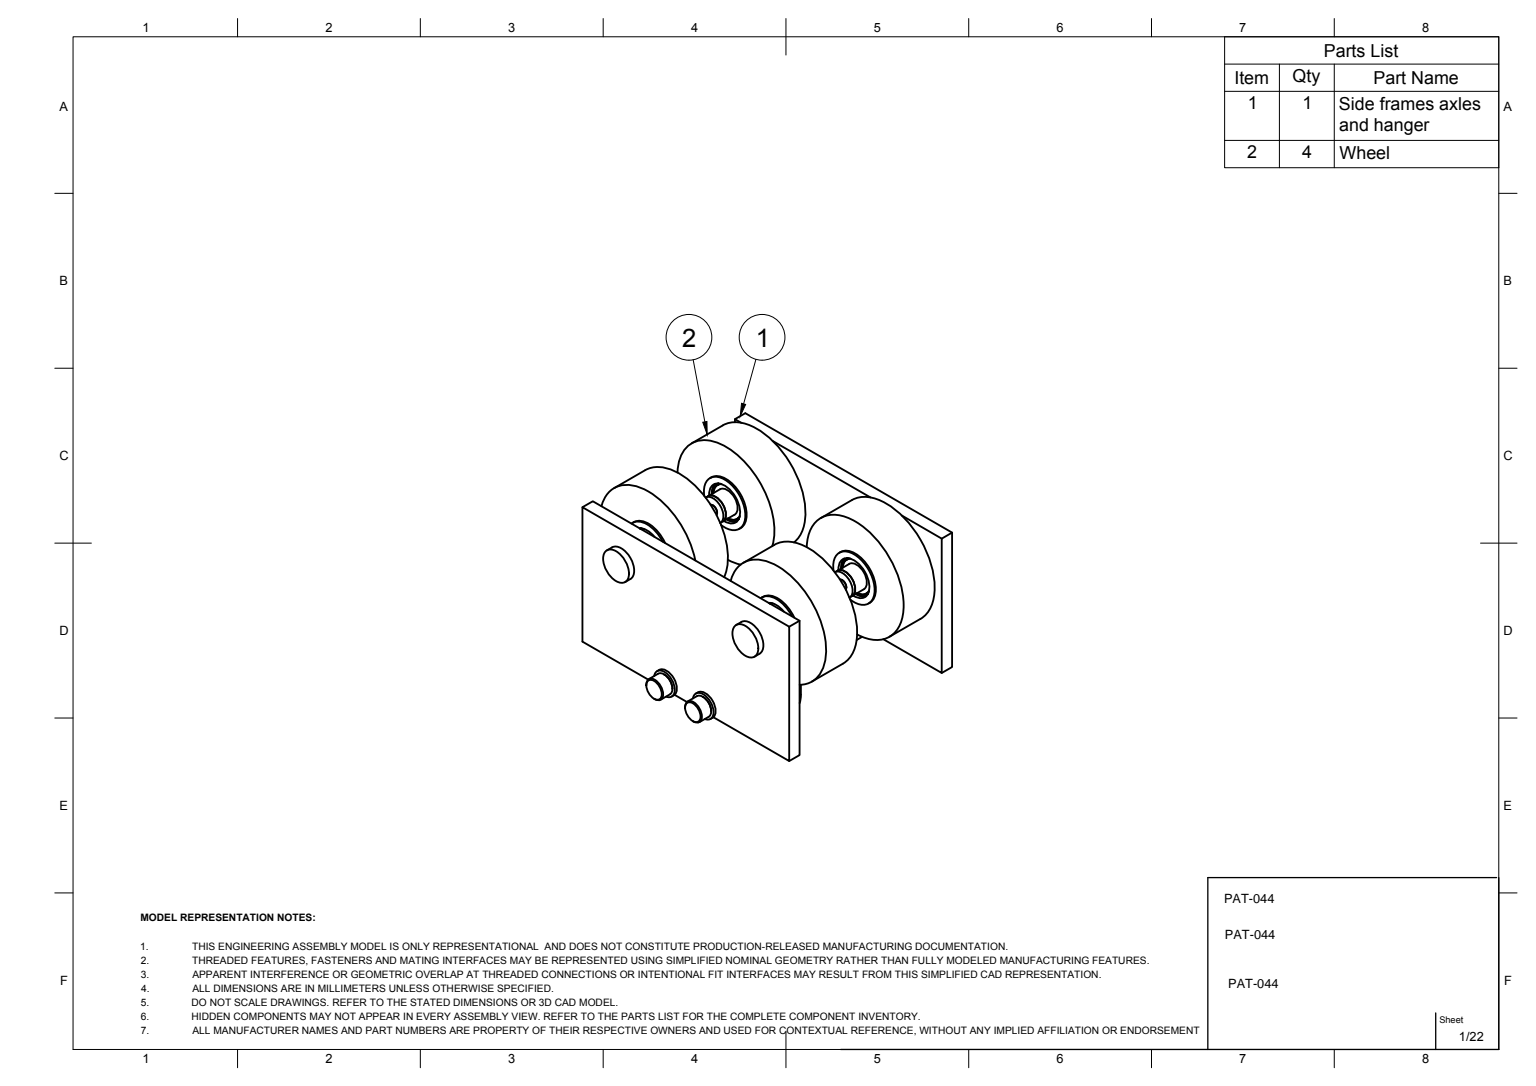
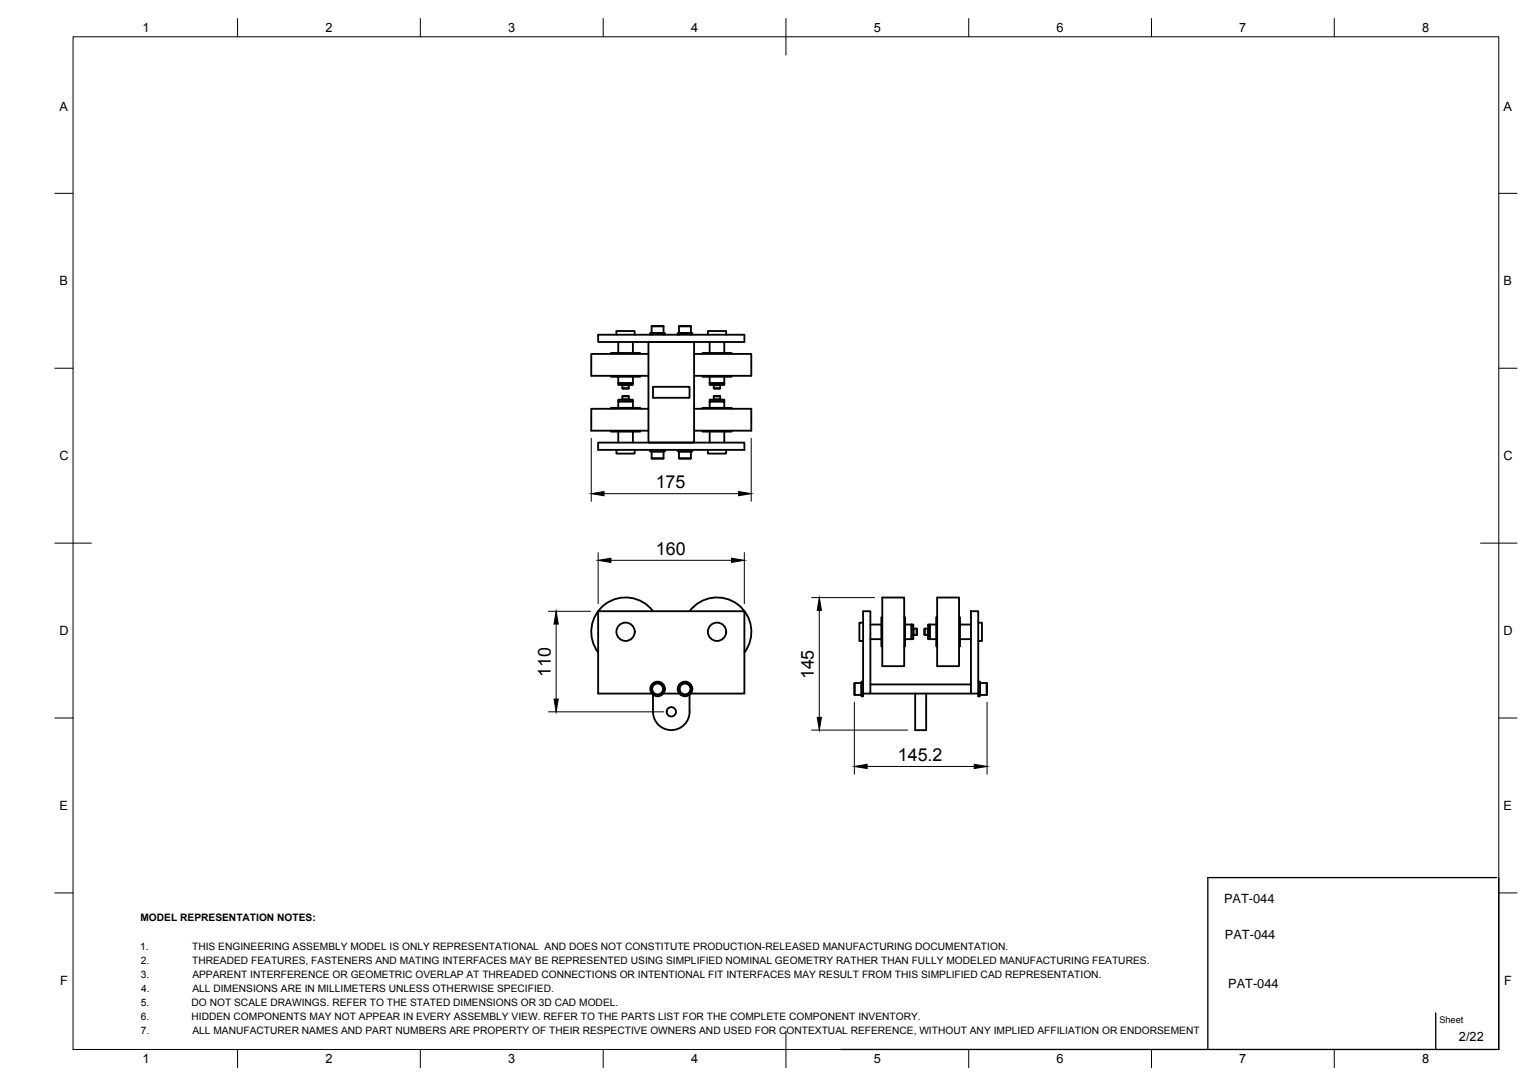
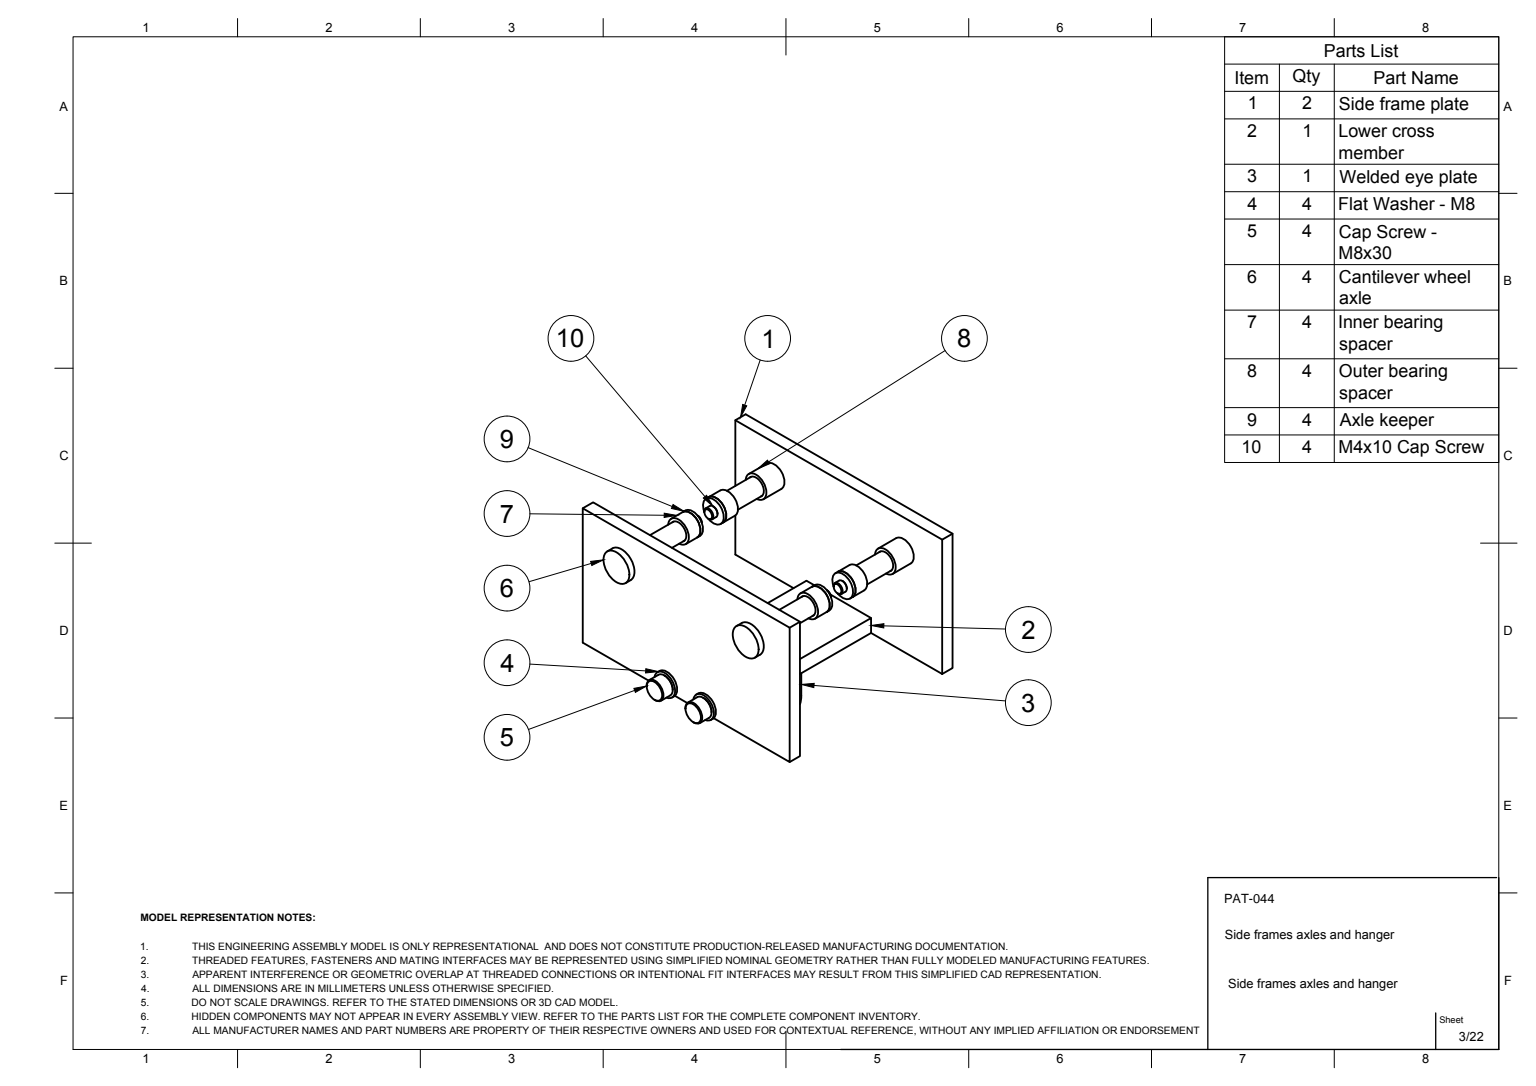
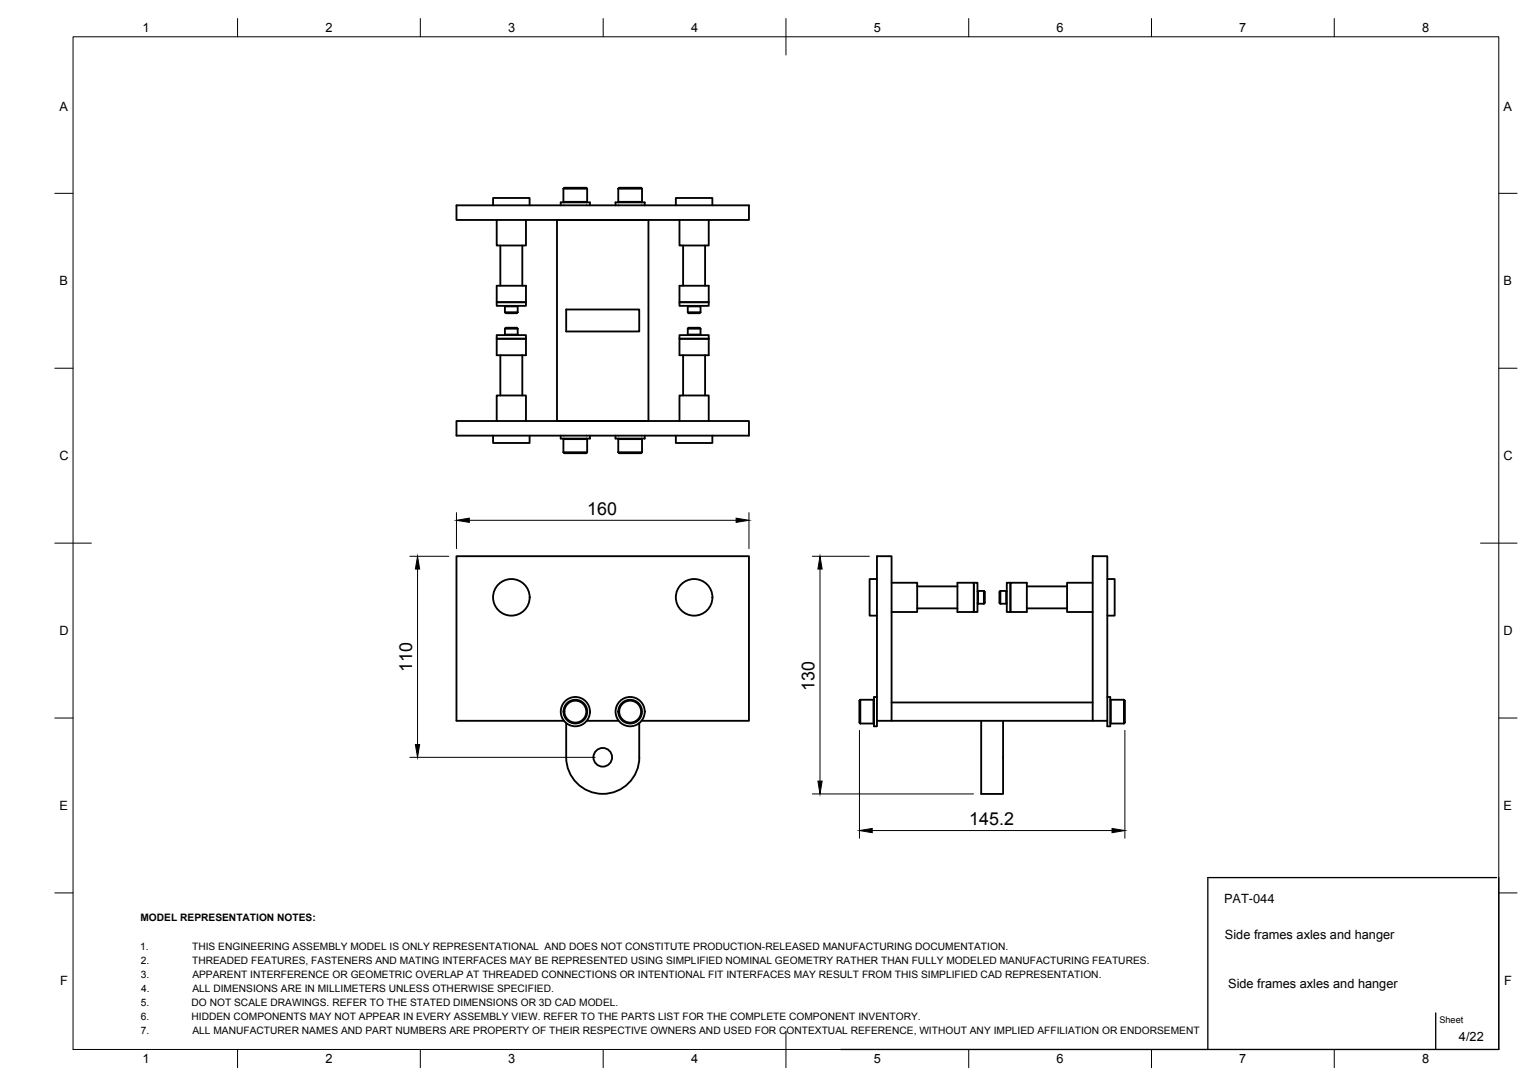
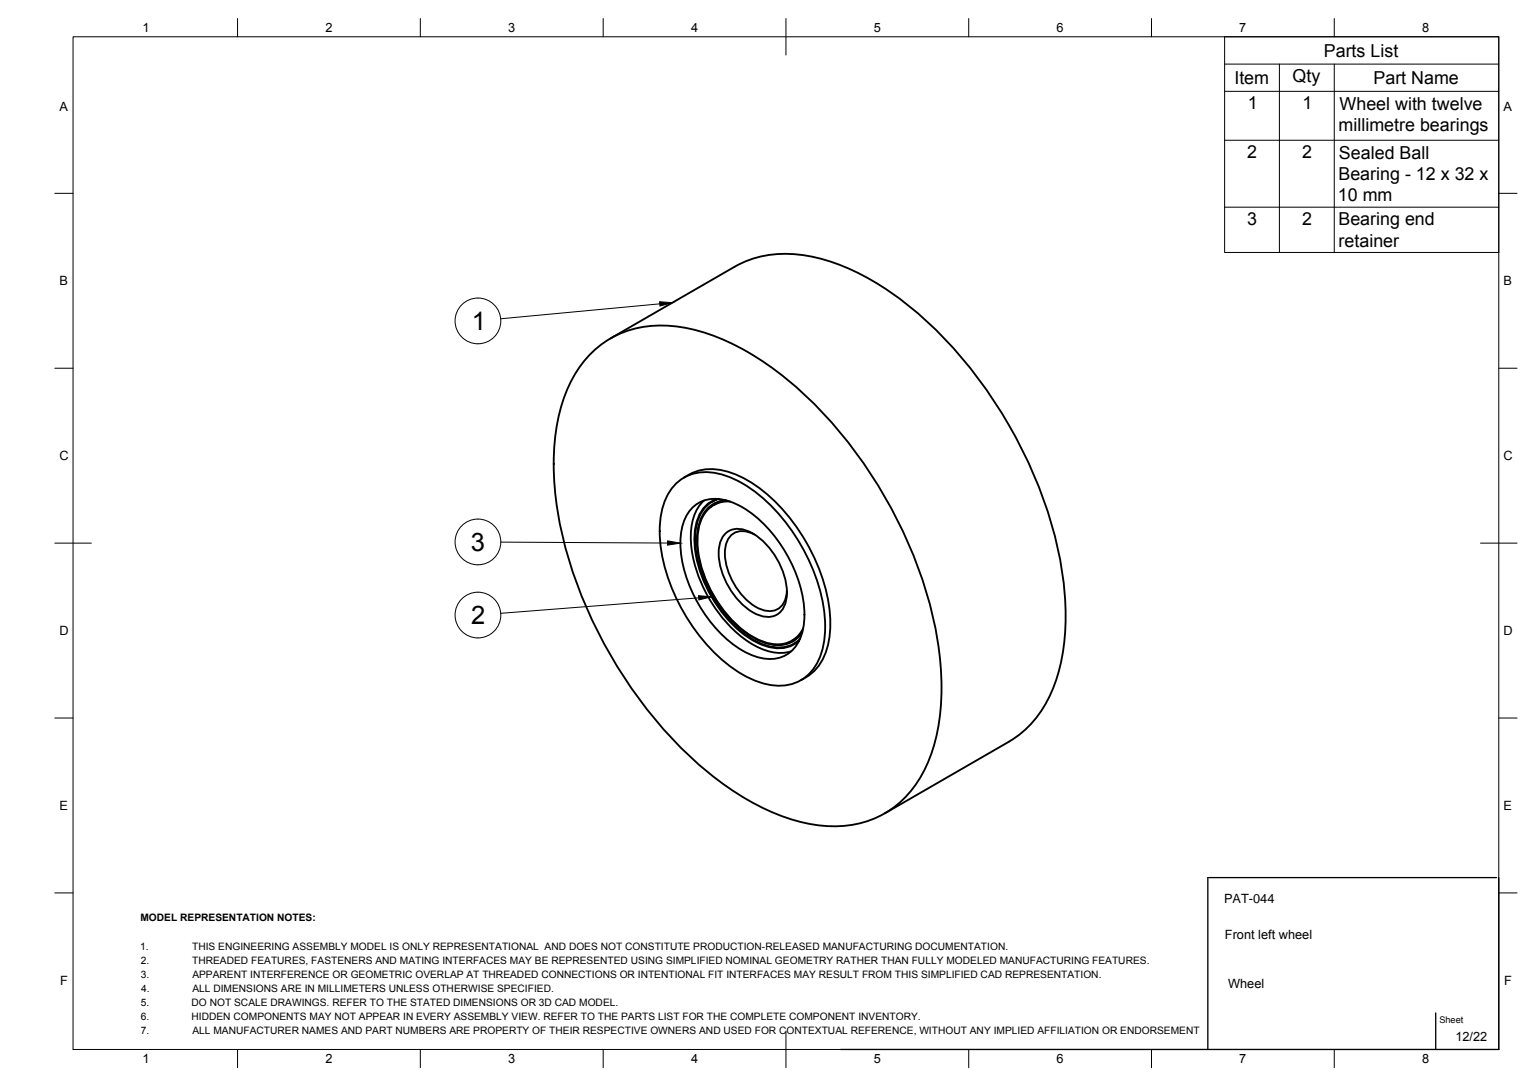
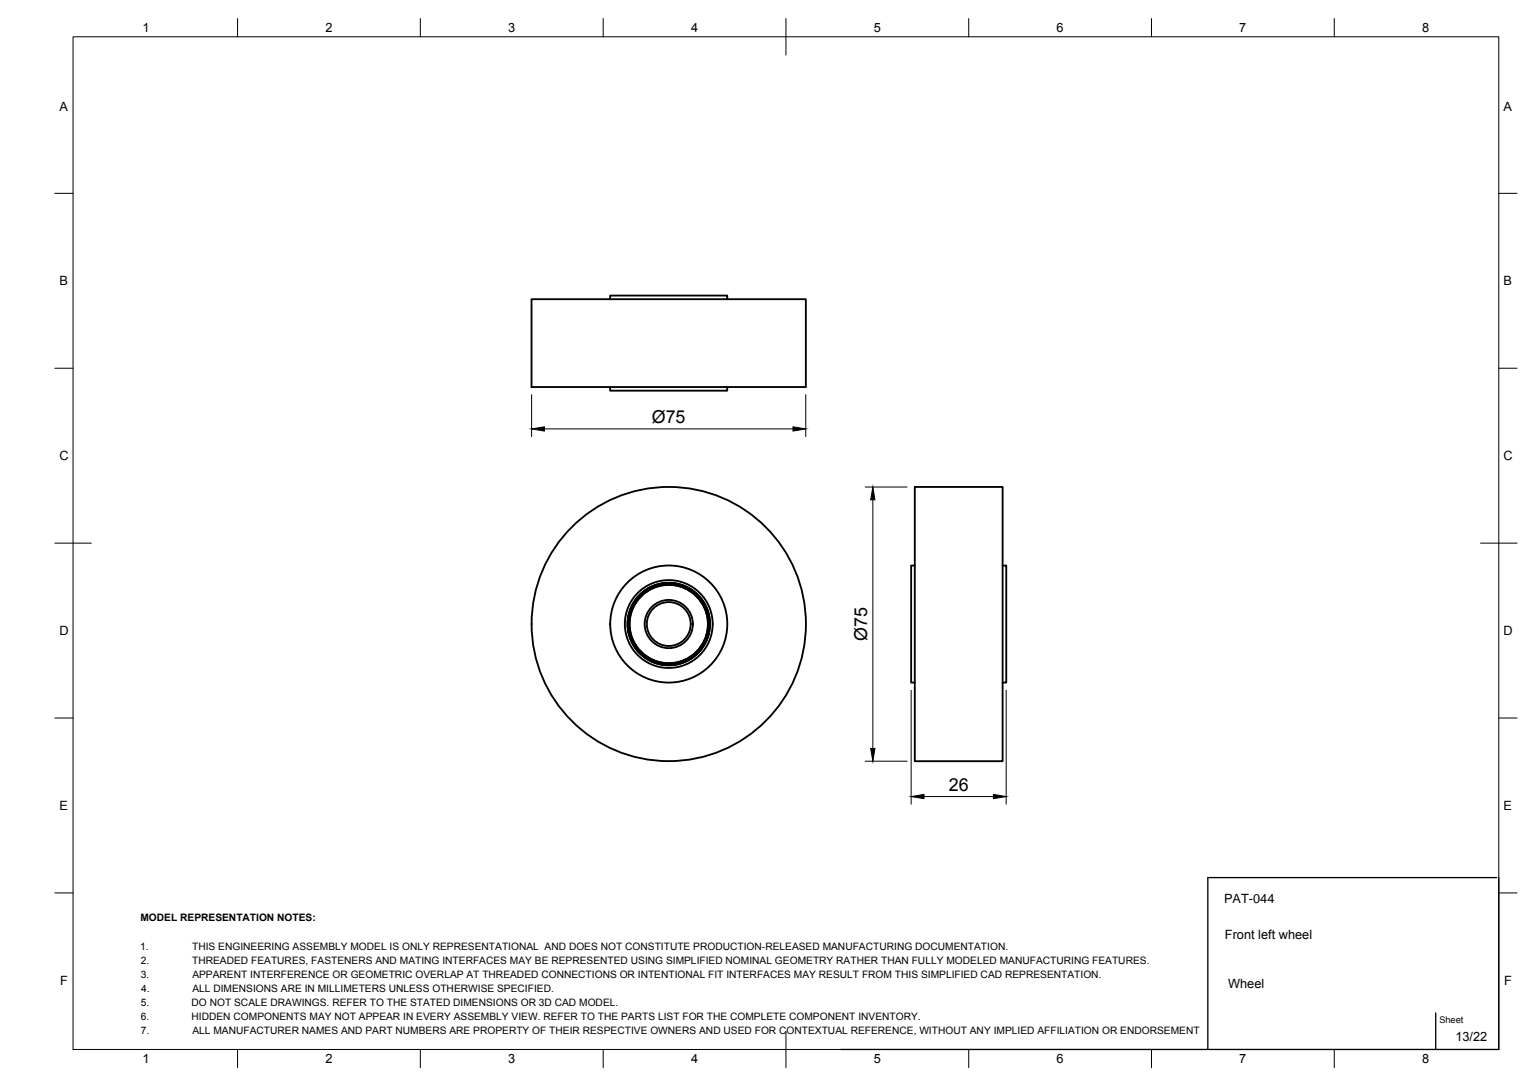
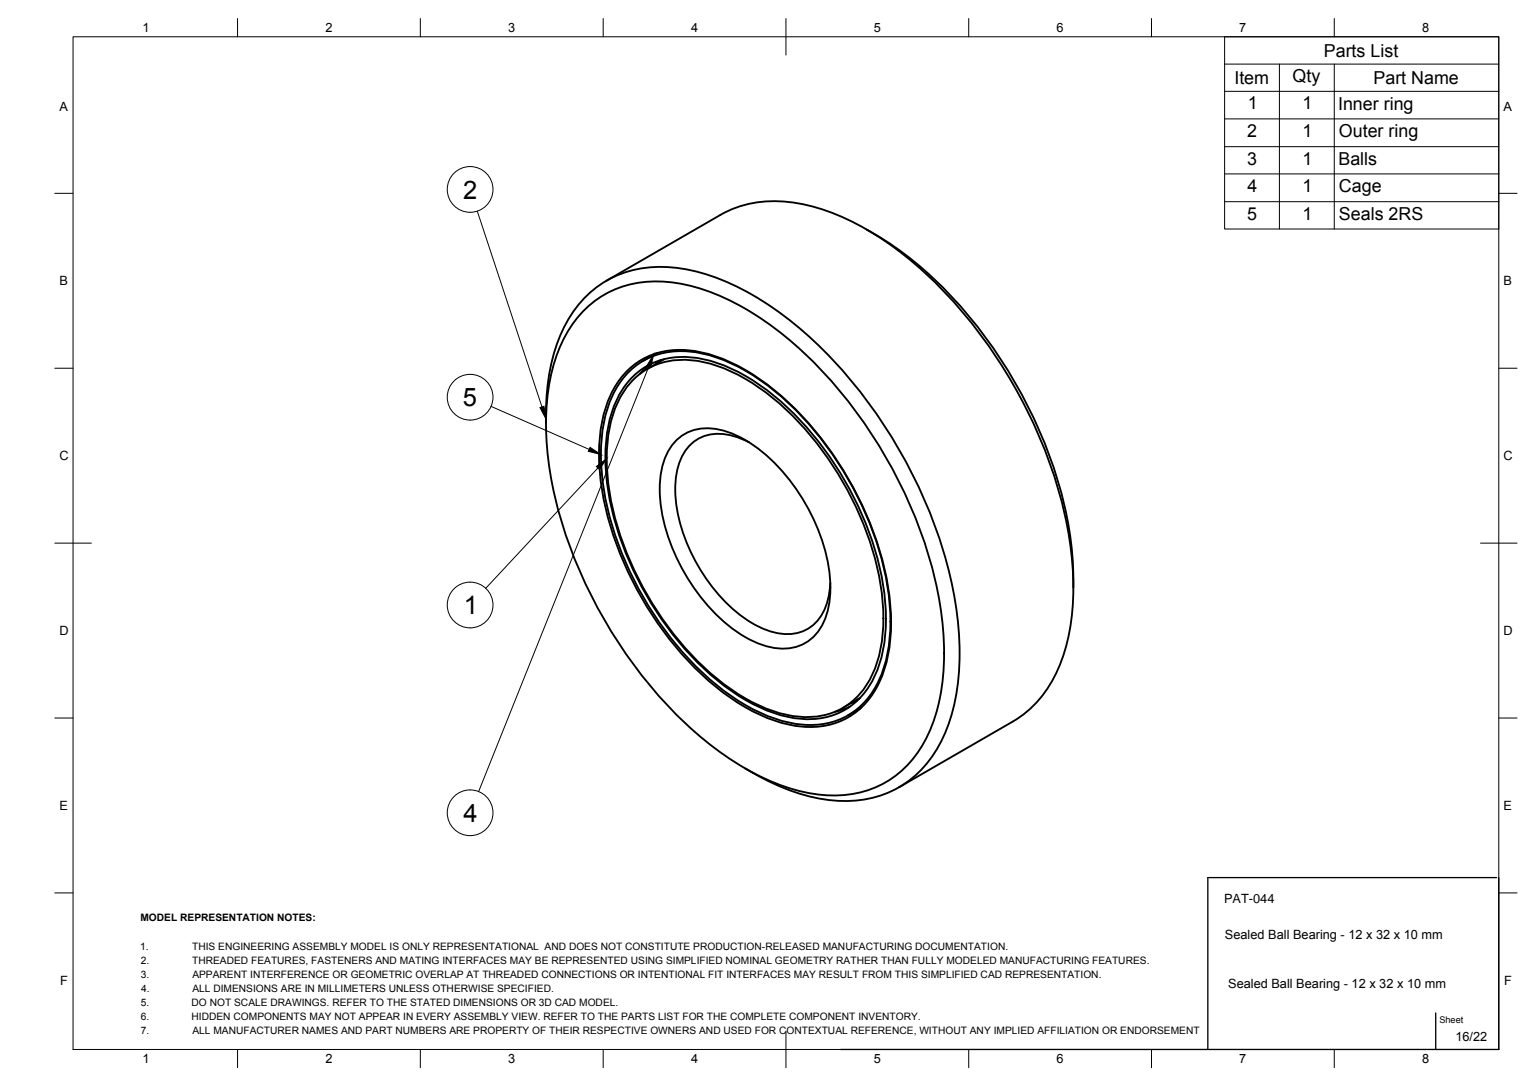
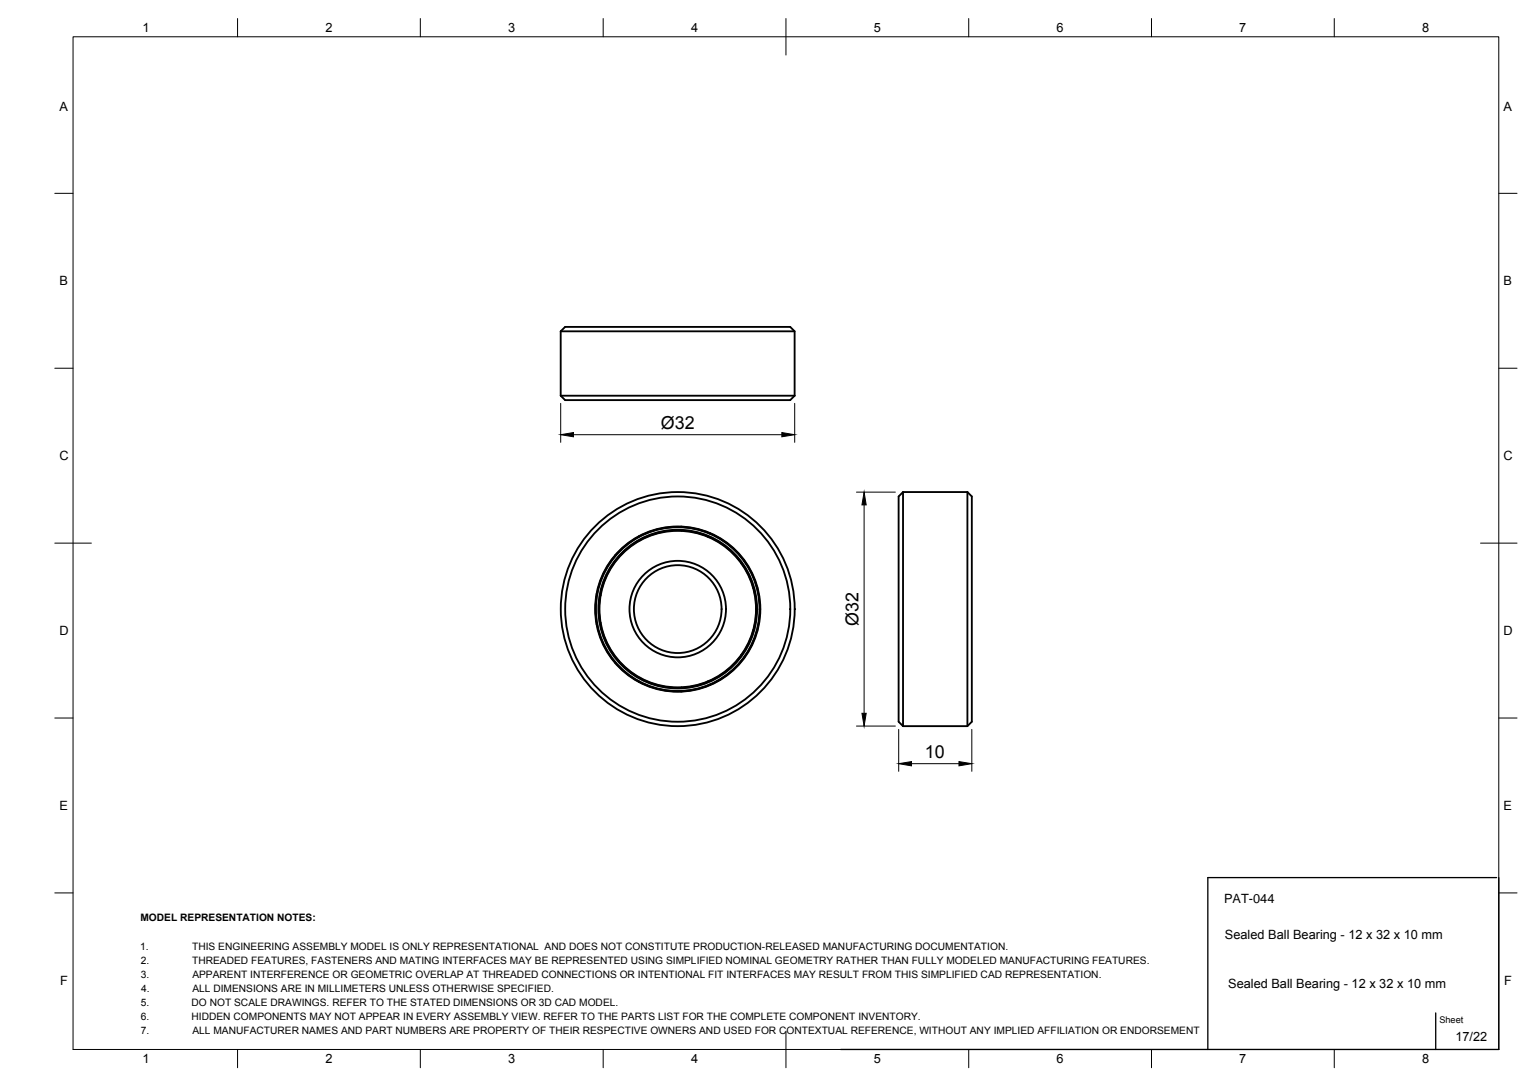
ISO-10303-21;
HEADER;
/* Generated by software containing ST-Developer
 * from STEP Tools, Inc. (www.steptools.com) 
 */

FILE_DESCRIPTION(
/* description */ ('Four-wheel beam trolley'),
/* implementation_level */ '2;1');

FILE_NAME(
/* name */ 'PAT-044',
/* time_stamp */ '2026-10-29T16:22:06-07:00',
/* author */ (''),
/* organization */ (''),
/* preprocessor_version */ 'ST-DEVELOPER v20.2',
/* originating_system */ 'Autodesk Translation Framework v15.17.0.0',
/* authorisation */ '');

FILE_SCHEMA (('AUTOMOTIVE_DESIGN { 1 0 10303 214 3 1 1 }'));
ENDSEC;

DATA;
#10=MECHANICAL_DESIGN_GEOMETRIC_PRESENTATION_REPRESENTATION('',(#278,#279,
#280,#281,#282,#283,#284,#285,#286,#287,#288,#289,#290,#291,#292,#293,#294,
#295,#296,#297,#298,#299,#300,#301),#4777);
#11=B_SPLINE_CURVE_WITH_KNOTS('',3,(#4287,#4288,#4289,#4290,#4291,#4292,
#4293,#4294,#4295,#4296,#4297,#4298,#4299,#4300,#4301,#4302,#4303,#4304,
#4305,#4306,#4307,#4308),.UNSPECIFIED.,.F.,.F.,(4,2,2,2,2,2,2,2,2,2,4),
(0.0591825211272536,0.157966726598481,0.236950089897721,0.315933453196962,
0.391576304923761,0.46721915665056,0.54286200837736,0.618504860104159,0.697488223403399,
0.77647158670264,0.875255792173867),.UNSPECIFIED.);
#12=B_SPLINE_CURVE_WITH_KNOTS('',3,(#4312,#4313,#4314,#4315,#4316,#4317,
#4318,#4319,#4320,#4321,#4322,#4323,#4324,#4325,#4326,#4327,#4328,#4329,
#4330,#4331,#4332,#4333),.UNSPECIFIED.,.F.,.F.,(4,2,2,2,2,2,2,2,2,2,4),
(0.0581119756758434,0.106553146291161,0.213106292582322,0.30849933801665,
0.386091982889075,0.4636846277615,0.541277272633925,0.61886991750635,0.714262962940678,
0.820816109231839,0.869257279847157),.UNSPECIFIED.);
#13=B_SPLINE_CURVE_WITH_KNOTS('',3,(#4339,#4340,#4341,#4342,#4343,#4344,
#4345,#4346,#4347,#4348,#4349,#4350,#4351,#4352,#4353,#4354,#4355,#4356,
#4357,#4358,#4359,#4360),.UNSPECIFIED.,.F.,.F.,(4,2,2,2,2,2,2,2,2,2,4),
(0.0581119756758434,0.106553146291161,0.213106292582322,0.30849933801665,
0.386091982889075,0.4636846277615,0.541277272633925,0.61886991750635,0.714262962940679,
0.820816109231839,0.869257279847157),.UNSPECIFIED.);
#14=B_SPLINE_CURVE_WITH_KNOTS('',3,(#4364,#4365,#4366,#4367,#4368,#4369,
#4370,#4371,#4372,#4373,#4374,#4375,#4376,#4377,#4378,#4379,#4380,#4381,
#4382,#4383,#4384,#4385),.UNSPECIFIED.,.F.,.F.,(4,2,2,2,2,2,2,2,2,2,4),
(0.0581119756758433,0.106553146291161,0.213106292582322,0.308499338016649,
0.386091982889075,0.4636846277615,0.541277272633925,0.61886991750635,0.714262962940678,
0.820816109231839,0.869257279847157),.UNSPECIFIED.);
#15=B_SPLINE_CURVE_WITH_KNOTS('',3,(#4394,#4395,#4396,#4397,#4398,#4399,
#4400,#4401,#4402,#4403,#4404,#4405,#4406,#4407,#4408,#4409,#4410,#4411,
#4412,#4413,#4414,#4415),.UNSPECIFIED.,.F.,.F.,(4,2,2,2,2,2,2,2,2,2,4),
(0.0581119756758433,0.106553146291161,0.213106292582322,0.30849933801665,
0.386091982889075,0.4636846277615,0.541277272633925,0.61886991750635,0.714262962940678,
0.820816109231839,0.869257279847157),.UNSPECIFIED.);
#16=B_SPLINE_CURVE_WITH_KNOTS('',3,(#4419,#4420,#4421,#4422,#4423,#4424,
#4425,#4426,#4427,#4428,#4429,#4430,#4431,#4432,#4433,#4434,#4435,#4436,
#4437,#4438,#4439,#4440),.UNSPECIFIED.,.F.,.F.,(4,2,2,2,2,2,2,2,2,2,4),
(0.0581119756758434,0.106553146291161,0.213106292582322,0.30849933801665,
0.386091982889075,0.4636846277615,0.541277272633925,0.61886991750635,0.714262962940678,
0.820816109231839,0.869257279847157),.UNSPECIFIED.);
#17=B_SPLINE_CURVE_WITH_KNOTS('',3,(#4444,#4445,#4446,#4447,#4448,#4449,
#4450,#4451,#4452,#4453,#4454,#4455,#4456,#4457,#4458,#4459,#4460,#4461,
#4462,#4463,#4464,#4465),.UNSPECIFIED.,.F.,.F.,(4,2,2,2,2,2,2,2,2,2,4),
(0.0581119756758434,0.106553146291161,0.213106292582322,0.30849933801665,
0.386091982889075,0.4636846277615,0.541277272633925,0.61886991750635,0.714262962940678,
0.820816109231839,0.869257279847157),.UNSPECIFIED.);
#18=B_SPLINE_CURVE_WITH_KNOTS('',3,(#4469,#4470,#4471,#4472,#4473,#4474,
#4475,#4476,#4477,#4478,#4479,#4480,#4481,#4482,#4483,#4484,#4485,#4486,
#4487,#4488,#4489,#4490),.UNSPECIFIED.,.F.,.F.,(4,2,2,2,2,2,2,2,2,2,4),
(0.0581119756758433,0.106553146291161,0.213106292582322,0.30849933801665,
0.386091982889075,0.4636846277615,0.541277272633925,0.61886991750635,0.714262962940678,
0.820816109231839,0.869257279847157),.UNSPECIFIED.);
#19=B_SPLINE_CURVE_WITH_KNOTS('',3,(#4498,#4499,#4500,#4501,#4502,#4503,
#4504,#4505,#4506,#4507,#4508,#4509,#4510,#4511,#4512,#4513,#4514,#4515,
#4516,#4517,#4518,#4519),.UNSPECIFIED.,.F.,.F.,(4,2,2,2,2,2,2,2,2,2,4),
(0.0591825211272536,0.157966726598481,0.236950089897721,0.315933453196962,
0.391576304923761,0.467219156650561,0.54286200837736,0.618504860104159,
0.697488223403399,0.77647158670264,0.875255792173867),.UNSPECIFIED.);
#20=B_SPLINE_CURVE_WITH_KNOTS('',3,(#4527,#4528,#4529,#4530,#4531,#4532,
#4533,#4534,#4535,#4536,#4537,#4538,#4539,#4540,#4541,#4542,#4543,#4544,
#4545,#4546,#4547,#4548),.UNSPECIFIED.,.F.,.F.,(4,2,2,2,2,2,2,2,2,2,4),
(0.0591825211272536,0.157966726598481,0.236950089897722,0.315933453196962,
0.391576304923761,0.467219156650561,0.54286200837736,0.618504860104159,
0.697488223403399,0.77647158670264,0.875255792173867),.UNSPECIFIED.);
#21=B_SPLINE_CURVE_WITH_KNOTS('',3,(#4558,#4559,#4560,#4561,#4562,#4563,
#4564,#4565,#4566,#4567,#4568,#4569,#4570,#4571,#4572,#4573,#4574,#4575,
#4576,#4577,#4578,#4579),.UNSPECIFIED.,.F.,.F.,(4,2,2,2,2,2,2,2,2,2,4),
(0.0591825211272536,0.157966726598481,0.236950089897721,0.315933453196962,
0.391576304923761,0.46721915665056,0.54286200837736,0.618504860104159,0.697488223403399,
0.77647158670264,0.875255792173867),.UNSPECIFIED.);
#22=B_SPLINE_CURVE_WITH_KNOTS('',3,(#4587,#4588,#4589,#4590,#4591,#4592,
#4593,#4594,#4595,#4596,#4597,#4598,#4599,#4600,#4601,#4602,#4603,#4604,
#4605,#4606,#4607,#4608),.UNSPECIFIED.,.F.,.F.,(4,2,2,2,2,2,2,2,2,2,4),
(0.0591825211272536,0.157966726598481,0.236950089897721,0.315933453196962,
0.391576304923761,0.46721915665056,0.542862008377359,0.618504860104159,
0.697488223403399,0.776471586702639,0.875255792173867),.UNSPECIFIED.);
#23=B_SPLINE_CURVE_WITH_KNOTS('',3,(#4616,#4617,#4618,#4619,#4620,#4621,
#4622,#4623,#4624,#4625,#4626,#4627,#4628,#4629,#4630,#4631,#4632,#4633,
#4634,#4635,#4636,#4637),.UNSPECIFIED.,.F.,.F.,(4,2,2,2,2,2,2,2,2,2,4),
(0.0591825211272536,0.157966726598481,0.236950089897721,0.315933453196962,
0.391576304923761,0.46721915665056,0.54286200837736,0.618504860104159,0.697488223403399,
0.77647158670264,0.875255792173867),.UNSPECIFIED.);
#24=B_SPLINE_CURVE_WITH_KNOTS('',3,(#4646,#4647,#4648,#4649,#4650,#4651,
#4652,#4653,#4654,#4655,#4656,#4657,#4658,#4659,#4660,#4661,#4662,#4663,
#4664,#4665,#4666,#4667),.UNSPECIFIED.,.F.,.F.,(4,2,2,2,2,2,2,2,2,2,4),
(0.0591825211272536,0.157966726598481,0.236950089897721,0.315933453196962,
0.391576304923761,0.46721915665056,0.542862008377359,0.618504860104159,
0.697488223403399,0.776471586702639,0.875255792173867),.UNSPECIFIED.);
#25=SPHERICAL_SURFACE('',#2827,0.29765);
#26=SPHERICAL_SURFACE('',#2829,0.29765);
#27=SPHERICAL_SURFACE('',#2831,0.29765);
#28=SPHERICAL_SURFACE('',#2833,0.29765);
#29=SPHERICAL_SURFACE('',#2835,0.29765);
#30=SPHERICAL_SURFACE('',#2837,0.29765);
#31=SPHERICAL_SURFACE('',#2839,0.29765);
#32=SPHERICAL_SURFACE('',#2842,0.309556);
#33=SPHERICAL_SURFACE('',#2858,0.309556);
#34=SPHERICAL_SURFACE('',#2863,0.309556);
#35=SPHERICAL_SURFACE('',#2869,0.309556);
#36=SPHERICAL_SURFACE('',#2874,0.309556);
#37=SPHERICAL_SURFACE('',#2879,0.309556);
#38=SPHERICAL_SURFACE('',#2887,0.309556);
#39=TOROIDAL_SURFACE('',#2787,1.1,0.309556);
#40=TOROIDAL_SURFACE('',#2807,1.1,0.309556);
#41=ITEM_DEFINED_TRANSFORMATION($,$,#2604,#2735);
#42=ITEM_DEFINED_TRANSFORMATION($,$,#2581,#2736);
#43=ITEM_DEFINED_TRANSFORMATION($,$,#2604,#2737);
#44=ITEM_DEFINED_TRANSFORMATION($,$,#2623,#2738);
#45=ITEM_DEFINED_TRANSFORMATION($,$,#2635,#2739);
#46=ITEM_DEFINED_TRANSFORMATION($,$,#2644,#2740);
#47=ITEM_DEFINED_TRANSFORMATION($,$,#2635,#2741);
#48=ITEM_DEFINED_TRANSFORMATION($,$,#2644,#2742);
#49=ITEM_DEFINED_TRANSFORMATION($,$,#2670,#2743);
#50=ITEM_DEFINED_TRANSFORMATION($,$,#2684,#2744);
#51=ITEM_DEFINED_TRANSFORMATION($,$,#2693,#2745);
#52=ITEM_DEFINED_TRANSFORMATION($,$,#2702,#2746);
#53=ITEM_DEFINED_TRANSFORMATION($,$,#2711,#2747);
#54=ITEM_DEFINED_TRANSFORMATION($,$,#2670,#2748);
#55=ITEM_DEFINED_TRANSFORMATION($,$,#2684,#2749);
#56=ITEM_DEFINED_TRANSFORMATION($,$,#2693,#2750);
#57=ITEM_DEFINED_TRANSFORMATION($,$,#2702,#2751);
#58=ITEM_DEFINED_TRANSFORMATION($,$,#2711,#2752);
#59=ITEM_DEFINED_TRANSFORMATION($,$,#2635,#2753);
#60=ITEM_DEFINED_TRANSFORMATION($,$,#2644,#2754);
#61=ITEM_DEFINED_TRANSFORMATION($,$,#2635,#2755);
#62=ITEM_DEFINED_TRANSFORMATION($,$,#2644,#2756);
#63=ITEM_DEFINED_TRANSFORMATION($,$,#2670,#2757);
#64=ITEM_DEFINED_TRANSFORMATION($,$,#2684,#2758);
#65=ITEM_DEFINED_TRANSFORMATION($,$,#2693,#2759);
#66=ITEM_DEFINED_TRANSFORMATION($,$,#2702,#2760);
#67=ITEM_DEFINED_TRANSFORMATION($,$,#2711,#2761);
#68=ITEM_DEFINED_TRANSFORMATION($,$,#2670,#2762);
#69=ITEM_DEFINED_TRANSFORMATION($,$,#2684,#2763);
#70=ITEM_DEFINED_TRANSFORMATION($,$,#2693,#2764);
#71=ITEM_DEFINED_TRANSFORMATION($,$,#2702,#2765);
#72=ITEM_DEFINED_TRANSFORMATION($,$,#2711,#2766);
#73=ITEM_DEFINED_TRANSFORMATION($,$,#2786,#2908);
#74=ITEM_DEFINED_TRANSFORMATION($,$,#2806,#2909);
#75=ITEM_DEFINED_TRANSFORMATION($,$,#2826,#2910);
#76=ITEM_DEFINED_TRANSFORMATION($,$,#2841,#2911);
#77=ITEM_DEFINED_TRANSFORMATION($,$,#2891,#2912);
#78=ITEM_DEFINED_TRANSFORMATION($,$,#2768,#2922);
#79=ITEM_DEFINED_TRANSFORMATION($,$,#2785,#2923);
#80=ITEM_DEFINED_TRANSFORMATION($,$,#2785,#2924);
#81=ITEM_DEFINED_TRANSFORMATION($,$,#2913,#2925);
#82=ITEM_DEFINED_TRANSFORMATION($,$,#2913,#2926);
#83=ITEM_DEFINED_TRANSFORMATION($,$,#2580,#2927);
#84=ITEM_DEFINED_TRANSFORMATION($,$,#2767,#2928);
#85=ITEM_DEFINED_TRANSFORMATION($,$,#2767,#2929);
#86=ITEM_DEFINED_TRANSFORMATION($,$,#2767,#2930);
#87=ITEM_DEFINED_TRANSFORMATION($,$,#2767,#2931);
#88=(
REPRESENTATION_RELATIONSHIP($,$,#4874,#4872)
REPRESENTATION_RELATIONSHIP_WITH_TRANSFORMATION(#41)
SHAPE_REPRESENTATION_RELATIONSHIP()
);
#89=(
REPRESENTATION_RELATIONSHIP($,$,#4873,#4872)
REPRESENTATION_RELATIONSHIP_WITH_TRANSFORMATION(#42)
SHAPE_REPRESENTATION_RELATIONSHIP()
);
#90=(
REPRESENTATION_RELATIONSHIP($,$,#4874,#4872)
REPRESENTATION_RELATIONSHIP_WITH_TRANSFORMATION(#43)
SHAPE_REPRESENTATION_RELATIONSHIP()
);
#91=(
REPRESENTATION_RELATIONSHIP($,$,#4875,#4872)
REPRESENTATION_RELATIONSHIP_WITH_TRANSFORMATION(#44)
SHAPE_REPRESENTATION_RELATIONSHIP()
);
#92=(
REPRESENTATION_RELATIONSHIP($,$,#4876,#4872)
REPRESENTATION_RELATIONSHIP_WITH_TRANSFORMATION(#45)
SHAPE_REPRESENTATION_RELATIONSHIP()
);
#93=(
REPRESENTATION_RELATIONSHIP($,$,#4877,#4872)
REPRESENTATION_RELATIONSHIP_WITH_TRANSFORMATION(#46)
SHAPE_REPRESENTATION_RELATIONSHIP()
);
#94=(
REPRESENTATION_RELATIONSHIP($,$,#4876,#4872)
REPRESENTATION_RELATIONSHIP_WITH_TRANSFORMATION(#47)
SHAPE_REPRESENTATION_RELATIONSHIP()
);
#95=(
REPRESENTATION_RELATIONSHIP($,$,#4877,#4872)
REPRESENTATION_RELATIONSHIP_WITH_TRANSFORMATION(#48)
SHAPE_REPRESENTATION_RELATIONSHIP()
);
#96=(
REPRESENTATION_RELATIONSHIP($,$,#4878,#4872)
REPRESENTATION_RELATIONSHIP_WITH_TRANSFORMATION(#49)
SHAPE_REPRESENTATION_RELATIONSHIP()
);
#97=(
REPRESENTATION_RELATIONSHIP($,$,#4879,#4872)
REPRESENTATION_RELATIONSHIP_WITH_TRANSFORMATION(#50)
SHAPE_REPRESENTATION_RELATIONSHIP()
);
#98=(
REPRESENTATION_RELATIONSHIP($,$,#4880,#4872)
REPRESENTATION_RELATIONSHIP_WITH_TRANSFORMATION(#51)
SHAPE_REPRESENTATION_RELATIONSHIP()
);
#99=(
REPRESENTATION_RELATIONSHIP($,$,#4881,#4872)
REPRESENTATION_RELATIONSHIP_WITH_TRANSFORMATION(#52)
SHAPE_REPRESENTATION_RELATIONSHIP()
);
#100=(
REPRESENTATION_RELATIONSHIP($,$,#4882,#4872)
REPRESENTATION_RELATIONSHIP_WITH_TRANSFORMATION(#53)
SHAPE_REPRESENTATION_RELATIONSHIP()
);
#101=(
REPRESENTATION_RELATIONSHIP($,$,#4878,#4872)
REPRESENTATION_RELATIONSHIP_WITH_TRANSFORMATION(#54)
SHAPE_REPRESENTATION_RELATIONSHIP()
);
#102=(
REPRESENTATION_RELATIONSHIP($,$,#4879,#4872)
REPRESENTATION_RELATIONSHIP_WITH_TRANSFORMATION(#55)
SHAPE_REPRESENTATION_RELATIONSHIP()
);
#103=(
REPRESENTATION_RELATIONSHIP($,$,#4880,#4872)
REPRESENTATION_RELATIONSHIP_WITH_TRANSFORMATION(#56)
SHAPE_REPRESENTATION_RELATIONSHIP()
);
#104=(
REPRESENTATION_RELATIONSHIP($,$,#4881,#4872)
REPRESENTATION_RELATIONSHIP_WITH_TRANSFORMATION(#57)
SHAPE_REPRESENTATION_RELATIONSHIP()
);
#105=(
REPRESENTATION_RELATIONSHIP($,$,#4882,#4872)
REPRESENTATION_RELATIONSHIP_WITH_TRANSFORMATION(#58)
SHAPE_REPRESENTATION_RELATIONSHIP()
);
#106=(
REPRESENTATION_RELATIONSHIP($,$,#4876,#4872)
REPRESENTATION_RELATIONSHIP_WITH_TRANSFORMATION(#59)
SHAPE_REPRESENTATION_RELATIONSHIP()
);
#107=(
REPRESENTATION_RELATIONSHIP($,$,#4877,#4872)
REPRESENTATION_RELATIONSHIP_WITH_TRANSFORMATION(#60)
SHAPE_REPRESENTATION_RELATIONSHIP()
);
#108=(
REPRESENTATION_RELATIONSHIP($,$,#4876,#4872)
REPRESENTATION_RELATIONSHIP_WITH_TRANSFORMATION(#61)
SHAPE_REPRESENTATION_RELATIONSHIP()
);
#109=(
REPRESENTATION_RELATIONSHIP($,$,#4877,#4872)
REPRESENTATION_RELATIONSHIP_WITH_TRANSFORMATION(#62)
SHAPE_REPRESENTATION_RELATIONSHIP()
);
#110=(
REPRESENTATION_RELATIONSHIP($,$,#4878,#4872)
REPRESENTATION_RELATIONSHIP_WITH_TRANSFORMATION(#63)
SHAPE_REPRESENTATION_RELATIONSHIP()
);
#111=(
REPRESENTATION_RELATIONSHIP($,$,#4879,#4872)
REPRESENTATION_RELATIONSHIP_WITH_TRANSFORMATION(#64)
SHAPE_REPRESENTATION_RELATIONSHIP()
);
#112=(
REPRESENTATION_RELATIONSHIP($,$,#4880,#4872)
REPRESENTATION_RELATIONSHIP_WITH_TRANSFORMATION(#65)
SHAPE_REPRESENTATION_RELATIONSHIP()
);
#113=(
REPRESENTATION_RELATIONSHIP($,$,#4881,#4872)
REPRESENTATION_RELATIONSHIP_WITH_TRANSFORMATION(#66)
SHAPE_REPRESENTATION_RELATIONSHIP()
);
#114=(
REPRESENTATION_RELATIONSHIP($,$,#4882,#4872)
REPRESENTATION_RELATIONSHIP_WITH_TRANSFORMATION(#67)
SHAPE_REPRESENTATION_RELATIONSHIP()
);
#115=(
REPRESENTATION_RELATIONSHIP($,$,#4878,#4872)
REPRESENTATION_RELATIONSHIP_WITH_TRANSFORMATION(#68)
SHAPE_REPRESENTATION_RELATIONSHIP()
);
#116=(
REPRESENTATION_RELATIONSHIP($,$,#4879,#4872)
REPRESENTATION_RELATIONSHIP_WITH_TRANSFORMATION(#69)
SHAPE_REPRESENTATION_RELATIONSHIP()
);
#117=(
REPRESENTATION_RELATIONSHIP($,$,#4880,#4872)
REPRESENTATION_RELATIONSHIP_WITH_TRANSFORMATION(#70)
SHAPE_REPRESENTATION_RELATIONSHIP()
);
#118=(
REPRESENTATION_RELATIONSHIP($,$,#4881,#4872)
REPRESENTATION_RELATIONSHIP_WITH_TRANSFORMATION(#71)
SHAPE_REPRESENTATION_RELATIONSHIP()
);
#119=(
REPRESENTATION_RELATIONSHIP($,$,#4882,#4872)
REPRESENTATION_RELATIONSHIP_WITH_TRANSFORMATION(#72)
SHAPE_REPRESENTATION_RELATIONSHIP()
);
#120=(
REPRESENTATION_RELATIONSHIP($,$,#4886,#4885)
REPRESENTATION_RELATIONSHIP_WITH_TRANSFORMATION(#73)
SHAPE_REPRESENTATION_RELATIONSHIP()
);
#121=(
REPRESENTATION_RELATIONSHIP($,$,#4887,#4885)
REPRESENTATION_RELATIONSHIP_WITH_TRANSFORMATION(#74)
SHAPE_REPRESENTATION_RELATIONSHIP()
);
#122=(
REPRESENTATION_RELATIONSHIP($,$,#4888,#4885)
REPRESENTATION_RELATIONSHIP_WITH_TRANSFORMATION(#75)
SHAPE_REPRESENTATION_RELATIONSHIP()
);
#123=(
REPRESENTATION_RELATIONSHIP($,$,#4889,#4885)
REPRESENTATION_RELATIONSHIP_WITH_TRANSFORMATION(#76)
SHAPE_REPRESENTATION_RELATIONSHIP()
);
#124=(
REPRESENTATION_RELATIONSHIP($,$,#4890,#4885)
REPRESENTATION_RELATIONSHIP_WITH_TRANSFORMATION(#77)
SHAPE_REPRESENTATION_RELATIONSHIP()
);
#125=(
REPRESENTATION_RELATIONSHIP($,$,#4884,#4883)
REPRESENTATION_RELATIONSHIP_WITH_TRANSFORMATION(#78)
SHAPE_REPRESENTATION_RELATIONSHIP()
);
#126=(
REPRESENTATION_RELATIONSHIP($,$,#4885,#4883)
REPRESENTATION_RELATIONSHIP_WITH_TRANSFORMATION(#79)
SHAPE_REPRESENTATION_RELATIONSHIP()
);
#127=(
REPRESENTATION_RELATIONSHIP($,$,#4885,#4883)
REPRESENTATION_RELATIONSHIP_WITH_TRANSFORMATION(#80)
SHAPE_REPRESENTATION_RELATIONSHIP()
);
#128=(
REPRESENTATION_RELATIONSHIP($,$,#4891,#4883)
REPRESENTATION_RELATIONSHIP_WITH_TRANSFORMATION(#81)
SHAPE_REPRESENTATION_RELATIONSHIP()
);
#129=(
REPRESENTATION_RELATIONSHIP($,$,#4891,#4883)
REPRESENTATION_RELATIONSHIP_WITH_TRANSFORMATION(#82)
SHAPE_REPRESENTATION_RELATIONSHIP()
);
#130=(
REPRESENTATION_RELATIONSHIP($,$,#4872,#4871)
REPRESENTATION_RELATIONSHIP_WITH_TRANSFORMATION(#83)
SHAPE_REPRESENTATION_RELATIONSHIP()
);
#131=(
REPRESENTATION_RELATIONSHIP($,$,#4883,#4871)
REPRESENTATION_RELATIONSHIP_WITH_TRANSFORMATION(#84)
SHAPE_REPRESENTATION_RELATIONSHIP()
);
#132=(
REPRESENTATION_RELATIONSHIP($,$,#4883,#4871)
REPRESENTATION_RELATIONSHIP_WITH_TRANSFORMATION(#85)
SHAPE_REPRESENTATION_RELATIONSHIP()
);
#133=(
REPRESENTATION_RELATIONSHIP($,$,#4883,#4871)
REPRESENTATION_RELATIONSHIP_WITH_TRANSFORMATION(#86)
SHAPE_REPRESENTATION_RELATIONSHIP()
);
#134=(
REPRESENTATION_RELATIONSHIP($,$,#4883,#4871)
REPRESENTATION_RELATIONSHIP_WITH_TRANSFORMATION(#87)
SHAPE_REPRESENTATION_RELATIONSHIP()
);
#135=CONTEXT_DEPENDENT_SHAPE_REPRESENTATION(#88,#4815);
#136=CONTEXT_DEPENDENT_SHAPE_REPRESENTATION(#89,#4816);
#137=CONTEXT_DEPENDENT_SHAPE_REPRESENTATION(#90,#4817);
#138=CONTEXT_DEPENDENT_SHAPE_REPRESENTATION(#91,#4818);
#139=CONTEXT_DEPENDENT_SHAPE_REPRESENTATION(#92,#4819);
#140=CONTEXT_DEPENDENT_SHAPE_REPRESENTATION(#93,#4820);
#141=CONTEXT_DEPENDENT_SHAPE_REPRESENTATION(#94,#4821);
#142=CONTEXT_DEPENDENT_SHAPE_REPRESENTATION(#95,#4822);
#143=CONTEXT_DEPENDENT_SHAPE_REPRESENTATION(#96,#4823);
#144=CONTEXT_DEPENDENT_SHAPE_REPRESENTATION(#97,#4824);
#145=CONTEXT_DEPENDENT_SHAPE_REPRESENTATION(#98,#4825);
#146=CONTEXT_DEPENDENT_SHAPE_REPRESENTATION(#99,#4826);
#147=CONTEXT_DEPENDENT_SHAPE_REPRESENTATION(#100,#4827);
#148=CONTEXT_DEPENDENT_SHAPE_REPRESENTATION(#101,#4828);
#149=CONTEXT_DEPENDENT_SHAPE_REPRESENTATION(#102,#4829);
#150=CONTEXT_DEPENDENT_SHAPE_REPRESENTATION(#103,#4830);
#151=CONTEXT_DEPENDENT_SHAPE_REPRESENTATION(#104,#4831);
#152=CONTEXT_DEPENDENT_SHAPE_REPRESENTATION(#105,#4832);
#153=CONTEXT_DEPENDENT_SHAPE_REPRESENTATION(#106,#4833);
#154=CONTEXT_DEPENDENT_SHAPE_REPRESENTATION(#107,#4834);
#155=CONTEXT_DEPENDENT_SHAPE_REPRESENTATION(#108,#4835);
#156=CONTEXT_DEPENDENT_SHAPE_REPRESENTATION(#109,#4836);
#157=CONTEXT_DEPENDENT_SHAPE_REPRESENTATION(#110,#4837);
#158=CONTEXT_DEPENDENT_SHAPE_REPRESENTATION(#111,#4838);
#159=CONTEXT_DEPENDENT_SHAPE_REPRESENTATION(#112,#4839);
#160=CONTEXT_DEPENDENT_SHAPE_REPRESENTATION(#113,#4840);
#161=CONTEXT_DEPENDENT_SHAPE_REPRESENTATION(#114,#4841);
#162=CONTEXT_DEPENDENT_SHAPE_REPRESENTATION(#115,#4842);
#163=CONTEXT_DEPENDENT_SHAPE_REPRESENTATION(#116,#4843);
#164=CONTEXT_DEPENDENT_SHAPE_REPRESENTATION(#117,#4844);
#165=CONTEXT_DEPENDENT_SHAPE_REPRESENTATION(#118,#4845);
#166=CONTEXT_DEPENDENT_SHAPE_REPRESENTATION(#119,#4846);
#167=CONTEXT_DEPENDENT_SHAPE_REPRESENTATION(#120,#4855);
#168=CONTEXT_DEPENDENT_SHAPE_REPRESENTATION(#121,#4856);
#169=CONTEXT_DEPENDENT_SHAPE_REPRESENTATION(#122,#4857);
#170=CONTEXT_DEPENDENT_SHAPE_REPRESENTATION(#123,#4858);
#171=CONTEXT_DEPENDENT_SHAPE_REPRESENTATION(#124,#4859);
#172=CONTEXT_DEPENDENT_SHAPE_REPRESENTATION(#125,#4861);
#173=CONTEXT_DEPENDENT_SHAPE_REPRESENTATION(#126,#4862);
#174=CONTEXT_DEPENDENT_SHAPE_REPRESENTATION(#127,#4863);
#175=CONTEXT_DEPENDENT_SHAPE_REPRESENTATION(#128,#4864);
#176=CONTEXT_DEPENDENT_SHAPE_REPRESENTATION(#129,#4865);
#177=CONTEXT_DEPENDENT_SHAPE_REPRESENTATION(#130,#4866);
#178=CONTEXT_DEPENDENT_SHAPE_REPRESENTATION(#131,#4867);
#179=CONTEXT_DEPENDENT_SHAPE_REPRESENTATION(#132,#4868);
#180=CONTEXT_DEPENDENT_SHAPE_REPRESENTATION(#133,#4869);
#181=CONTEXT_DEPENDENT_SHAPE_REPRESENTATION(#134,#4870);
#182=NEXT_ASSEMBLY_USAGE_OCCURRENCE('Side frame plate:1',
'Side frame plate:1','Side frame plate:1',#4894,#4896,
'Side frame plate:1');
#183=NEXT_ASSEMBLY_USAGE_OCCURRENCE('Lower cross member:1',
'Lower cross member:1','Lower cross member:1',#4894,#4895,
'Lower cross member:1');
#184=NEXT_ASSEMBLY_USAGE_OCCURRENCE('Side frame plate:2',
'Side frame plate:2','Side frame plate:2',#4894,#4896,
'Side frame plate:2');
#185=NEXT_ASSEMBLY_USAGE_OCCURRENCE('Welded eye plate:2',
'Welded eye plate:2','Welded eye plate:2',#4894,#4897,
'Welded eye plate:2');
#186=NEXT_ASSEMBLY_USAGE_OCCURRENCE('Flat Washer - M8:2',
'Flat Washer - M8:2','Flat Washer - M8:2',#4894,#4898,
'Flat Washer - M8:2');
#187=NEXT_ASSEMBLY_USAGE_OCCURRENCE('Cap Screw - M8x30:2',
'Cap Screw - M8x30:2','Cap Screw - M8x30:2',#4894,#4899,
'Cap Screw - M8x30:2');
#188=NEXT_ASSEMBLY_USAGE_OCCURRENCE('Flat Washer - M8:3',
'Flat Washer - M8:3','Flat Washer - M8:3',#4894,#4898,
'Flat Washer - M8:3');
#189=NEXT_ASSEMBLY_USAGE_OCCURRENCE('Cap Screw - M8x30:3',
'Cap Screw - M8x30:3','Cap Screw - M8x30:3',#4894,#4899,
'Cap Screw - M8x30:3');
#190=NEXT_ASSEMBLY_USAGE_OCCURRENCE('Cantilever wheel axle:2',
'Cantilever wheel axle:2','Cantilever wheel axle:2',#4894,#4900,
'Cantilever wheel axle:2');
#191=NEXT_ASSEMBLY_USAGE_OCCURRENCE('Inner bearing spacer:2',
'Inner bearing spacer:2','Inner bearing spacer:2',#4894,#4901,
'Inner bearing spacer:2');
#192=NEXT_ASSEMBLY_USAGE_OCCURRENCE('Outer bearing spacer:2',
'Outer bearing spacer:2','Outer bearing spacer:2',#4894,#4902,
'Outer bearing spacer:2');
#193=NEXT_ASSEMBLY_USAGE_OCCURRENCE('Axle keeper:2','Axle keeper:2',
'Axle keeper:2',#4894,#4903,'Axle keeper:2');
#194=NEXT_ASSEMBLY_USAGE_OCCURRENCE('M4x10 Cap Screw:2',
'M4x10 Cap Screw:2','M4x10 Cap Screw:2',#4894,#4904,'M4x10 Cap Screw:2');
#195=NEXT_ASSEMBLY_USAGE_OCCURRENCE('Cantilever wheel axle:3',
'Cantilever wheel axle:3','Cantilever wheel axle:3',#4894,#4900,
'Cantilever wheel axle:3');
#196=NEXT_ASSEMBLY_USAGE_OCCURRENCE('Inner bearing spacer:3',
'Inner bearing spacer:3','Inner bearing spacer:3',#4894,#4901,
'Inner bearing spacer:3');
#197=NEXT_ASSEMBLY_USAGE_OCCURRENCE('Outer bearing spacer:3',
'Outer bearing spacer:3','Outer bearing spacer:3',#4894,#4902,
'Outer bearing spacer:3');
#198=NEXT_ASSEMBLY_USAGE_OCCURRENCE('Axle keeper:3','Axle keeper:3',
'Axle keeper:3',#4894,#4903,'Axle keeper:3');
#199=NEXT_ASSEMBLY_USAGE_OCCURRENCE('M4x10 Cap Screw:3',
'M4x10 Cap Screw:3','M4x10 Cap Screw:3',#4894,#4904,'M4x10 Cap Screw:3');
#200=NEXT_ASSEMBLY_USAGE_OCCURRENCE('Flat Washer - M8:4',
'Flat Washer - M8:4','Flat Washer - M8:4',#4894,#4898,
'Flat Washer - M8:4');
#201=NEXT_ASSEMBLY_USAGE_OCCURRENCE('Cap Screw - M8x30:4',
'Cap Screw - M8x30:4','Cap Screw - M8x30:4',#4894,#4899,
'Cap Screw - M8x30:4');
#202=NEXT_ASSEMBLY_USAGE_OCCURRENCE('Flat Washer - M8:5',
'Flat Washer - M8:5','Flat Washer - M8:5',#4894,#4898,
'Flat Washer - M8:5');
#203=NEXT_ASSEMBLY_USAGE_OCCURRENCE('Cap Screw - M8x30:5',
'Cap Screw - M8x30:5','Cap Screw - M8x30:5',#4894,#4899,
'Cap Screw - M8x30:5');
#204=NEXT_ASSEMBLY_USAGE_OCCURRENCE('Cantilever wheel axle:4',
'Cantilever wheel axle:4','Cantilever wheel axle:4',#4894,#4900,
'Cantilever wheel axle:4');
#205=NEXT_ASSEMBLY_USAGE_OCCURRENCE('Inner bearing spacer:4',
'Inner bearing spacer:4','Inner bearing spacer:4',#4894,#4901,
'Inner bearing spacer:4');
#206=NEXT_ASSEMBLY_USAGE_OCCURRENCE('Outer bearing spacer:4',
'Outer bearing spacer:4','Outer bearing spacer:4',#4894,#4902,
'Outer bearing spacer:4');
#207=NEXT_ASSEMBLY_USAGE_OCCURRENCE('Axle keeper:4','Axle keeper:4',
'Axle keeper:4',#4894,#4903,'Axle keeper:4');
#208=NEXT_ASSEMBLY_USAGE_OCCURRENCE('M4x10 Cap Screw:4',
'M4x10 Cap Screw:4','M4x10 Cap Screw:4',#4894,#4904,'M4x10 Cap Screw:4');
#209=NEXT_ASSEMBLY_USAGE_OCCURRENCE('Cantilever wheel axle:5',
'Cantilever wheel axle:5','Cantilever wheel axle:5',#4894,#4900,
'Cantilever wheel axle:5');
#210=NEXT_ASSEMBLY_USAGE_OCCURRENCE('Inner bearing spacer:5',
'Inner bearing spacer:5','Inner bearing spacer:5',#4894,#4901,
'Inner bearing spacer:5');
#211=NEXT_ASSEMBLY_USAGE_OCCURRENCE('Outer bearing spacer:5',
'Outer bearing spacer:5','Outer bearing spacer:5',#4894,#4902,
'Outer bearing spacer:5');
#212=NEXT_ASSEMBLY_USAGE_OCCURRENCE('Axle keeper:5','Axle keeper:5',
'Axle keeper:5',#4894,#4903,'Axle keeper:5');
#213=NEXT_ASSEMBLY_USAGE_OCCURRENCE('M4x10 Cap Screw:5',
'M4x10 Cap Screw:5','M4x10 Cap Screw:5',#4894,#4904,'M4x10 Cap Screw:5');
#214=NEXT_ASSEMBLY_USAGE_OCCURRENCE('Inner ring:1','Inner ring:1',
'Inner ring:1',#4907,#4908,'Inner ring:1');
#215=NEXT_ASSEMBLY_USAGE_OCCURRENCE('Outer ring:1','Outer ring:1',
'Outer ring:1',#4907,#4909,'Outer ring:1');
#216=NEXT_ASSEMBLY_USAGE_OCCURRENCE('Balls:1','Balls:1','Balls:1',#4907,
#4910,'Balls:1');
#217=NEXT_ASSEMBLY_USAGE_OCCURRENCE('Cage:1','Cage:1','Cage:1',#4907,#4911,
'Cage:1');
#218=NEXT_ASSEMBLY_USAGE_OCCURRENCE('Seals 2RS:1','Seals 2RS:1',
'Seals 2RS:1',#4907,#4912,'Seals 2RS:1');
#219=NEXT_ASSEMBLY_USAGE_OCCURRENCE(
'Wheel with twelve millimetre bearings:2',
'Wheel with twelve millimetre bearings:2',
'Wheel with twelve millimetre bearings:2',#4905,#4906,
'Wheel with twelve millimetre bearings:2');
#220=NEXT_ASSEMBLY_USAGE_OCCURRENCE(
'Sealed Ball Bearing - 12 x 32 x 10 mm:2',
'Sealed Ball Bearing - 12 x 32 x 10 mm:2',
'Sealed Ball Bearing - 12 x 32 x 10 mm:2',#4905,#4907,
'Sealed Ball Bearing - 12 x 32 x 10 mm:2');
#221=NEXT_ASSEMBLY_USAGE_OCCURRENCE(
'Sealed Ball Bearing - 12 x 32 x 10 mm:3',
'Sealed Ball Bearing - 12 x 32 x 10 mm:3',
'Sealed Ball Bearing - 12 x 32 x 10 mm:3',#4905,#4907,
'Sealed Ball Bearing - 12 x 32 x 10 mm:3');
#222=NEXT_ASSEMBLY_USAGE_OCCURRENCE('Bearing end retainer:2',
'Bearing end retainer:2','Bearing end retainer:2',#4905,#4913,
'Bearing end retainer:2');
#223=NEXT_ASSEMBLY_USAGE_OCCURRENCE('Bearing end retainer:3',
'Bearing end retainer:3','Bearing end retainer:3',#4905,#4913,
'Bearing end retainer:3');
#224=NEXT_ASSEMBLY_USAGE_OCCURRENCE('Side frames axles and hanger:1',
'Side frames axles and hanger:1','Side frames axles and hanger:1',#4893,
#4894,'Side frames axles and hanger:1');
#225=NEXT_ASSEMBLY_USAGE_OCCURRENCE('Wheel:1','Wheel:1','Wheel:1',#4893,
#4905,'Wheel:1');
#226=NEXT_ASSEMBLY_USAGE_OCCURRENCE('Wheel:2','Wheel:2','Wheel:2',#4893,
#4905,'Wheel:2');
#227=NEXT_ASSEMBLY_USAGE_OCCURRENCE('Wheel:3','Wheel:3','Wheel:3',#4893,
#4905,'Wheel:3');
#228=NEXT_ASSEMBLY_USAGE_OCCURRENCE('Wheel:4','Wheel:4','Wheel:4',#4893,
#4905,'Wheel:4');
#229=ORIENTED_CLOSED_SHELL('',*,#2370,.F.);
#230=ORIENTED_CLOSED_SHELL('',*,#2375,.F.);
#231=CONICAL_SURFACE('',#2647,0.625,0.785398163397448);
#232=CONICAL_SURFACE('',#2651,0.635,0.785398163397449);
#233=CONICAL_SURFACE('',#2655,0.41,0.463647609000806);
#234=CONICAL_SURFACE('',#2659,0.36,0.785398163397448);
#235=CONICAL_SURFACE('',#2724,0.325,0.785398163397448);
#236=CONICAL_SURFACE('',#2728,0.335,0.785398163397448);
#237=CONICAL_SURFACE('',#2732,0.21,0.463647609000806);
#238=CONICAL_SURFACE('',#2798,0.63,0.785398163397448);
#239=CONICAL_SURFACE('',#2805,0.63,0.785398163397448);
#240=CONICAL_SURFACE('',#2818,1.57,0.785398163397449);
#241=CONICAL_SURFACE('',#2822,1.57,0.785398163397449);
#242=BREP_WITH_VOIDS('Body1',#2369,(#229));
#243=BREP_WITH_VOIDS('Body1',#2376,(#230));
#244=SHAPE_REPRESENTATION_RELATIONSHIP('SRR','None',#4873,#261);
#245=SHAPE_REPRESENTATION_RELATIONSHIP('SRR','None',#4874,#262);
#246=SHAPE_REPRESENTATION_RELATIONSHIP('SRR','None',#4875,#263);
#247=SHAPE_REPRESENTATION_RELATIONSHIP('SRR','None',#4876,#264);
#248=SHAPE_REPRESENTATION_RELATIONSHIP('SRR','None',#4877,#265);
#249=SHAPE_REPRESENTATION_RELATIONSHIP('SRR','None',#4878,#266);
#250=SHAPE_REPRESENTATION_RELATIONSHIP('SRR','None',#4879,#267);
#251=SHAPE_REPRESENTATION_RELATIONSHIP('SRR','None',#4880,#268);
#252=SHAPE_REPRESENTATION_RELATIONSHIP('SRR','None',#4881,#269);
#253=SHAPE_REPRESENTATION_RELATIONSHIP('SRR','None',#4882,#270);
#254=SHAPE_REPRESENTATION_RELATIONSHIP('SRR','None',#4884,#271);
#255=SHAPE_REPRESENTATION_RELATIONSHIP('SRR','None',#4886,#272);
#256=SHAPE_REPRESENTATION_RELATIONSHIP('SRR','None',#4887,#273);
#257=SHAPE_REPRESENTATION_RELATIONSHIP('SRR','None',#4888,#274);
#258=SHAPE_REPRESENTATION_RELATIONSHIP('SRR','None',#4889,#275);
#259=SHAPE_REPRESENTATION_RELATIONSHIP('SRR','None',#4890,#276);
#260=SHAPE_REPRESENTATION_RELATIONSHIP('SRR','None',#4891,#277);
#261=ADVANCED_BREP_SHAPE_REPRESENTATION('',(#302),#4758);
#262=ADVANCED_BREP_SHAPE_REPRESENTATION('',(#303),#4759);
#263=ADVANCED_BREP_SHAPE_REPRESENTATION('',(#304),#4760);
#264=ADVANCED_BREP_SHAPE_REPRESENTATION('',(#305),#4761);
#265=ADVANCED_BREP_SHAPE_REPRESENTATION('',(#242),#4762);
#266=ADVANCED_BREP_SHAPE_REPRESENTATION('',(#306),#4763);
#267=ADVANCED_BREP_SHAPE_REPRESENTATION('',(#307),#4764);
#268=ADVANCED_BREP_SHAPE_REPRESENTATION('',(#308),#4765);
#269=ADVANCED_BREP_SHAPE_REPRESENTATION('',(#309),#4766);
#270=ADVANCED_BREP_SHAPE_REPRESENTATION('',(#243),#4767);
#271=ADVANCED_BREP_SHAPE_REPRESENTATION('',(#310),#4769);
#272=ADVANCED_BREP_SHAPE_REPRESENTATION('',(#311),#4771);
#273=ADVANCED_BREP_SHAPE_REPRESENTATION('',(#312),#4772);
#274=ADVANCED_BREP_SHAPE_REPRESENTATION('',(#313,#314,#315,#316,#317,#318,
#319),#4773);
#275=ADVANCED_BREP_SHAPE_REPRESENTATION('',(#320),#4774);
#276=ADVANCED_BREP_SHAPE_REPRESENTATION('',(#321,#322),#4775);
#277=ADVANCED_BREP_SHAPE_REPRESENTATION('',(#323),#4776);
#278=STYLED_ITEM('',(#5049),#302);
#279=STYLED_ITEM('',(#5035),#303);
#280=STYLED_ITEM('',(#5049),#304);
#281=STYLED_ITEM('',(#5063),#305);
#282=STYLED_ITEM('',(#5063),#242);
#283=STYLED_ITEM('',(#5056),#306);
#284=STYLED_ITEM('',(#5056),#307);
#285=STYLED_ITEM('',(#5056),#308);
#286=STYLED_ITEM('',(#5056),#309);
#287=STYLED_ITEM('',(#5063),#243);
#288=STYLED_ITEM('',(#5056),#310);
#289=STYLED_ITEM('',(#5056),#311);
#290=STYLED_ITEM('',(#5056),#312);
#291=STYLED_ITEM('',(#5056),#313);
#292=STYLED_ITEM('',(#5056),#314);
#293=STYLED_ITEM('',(#5056),#315);
#294=STYLED_ITEM('',(#5056),#316);
#295=STYLED_ITEM('',(#5056),#317);
#296=STYLED_ITEM('',(#5056),#318);
#297=STYLED_ITEM('',(#5056),#319);
#298=STYLED_ITEM('',(#5056),#320);
#299=STYLED_ITEM('',(#5056),#321);
#300=STYLED_ITEM('',(#5056),#322);
#301=STYLED_ITEM('',(#5056),#323);
#302=MANIFOLD_SOLID_BREP('Body1',#2365);
#303=MANIFOLD_SOLID_BREP('Body1',#2366);
#304=MANIFOLD_SOLID_BREP('Body1',#2367);
#305=MANIFOLD_SOLID_BREP('Body1',#2368);
#306=MANIFOLD_SOLID_BREP('Body1',#2371);
#307=MANIFOLD_SOLID_BREP('Body1',#2372);
#308=MANIFOLD_SOLID_BREP('Body1',#2373);
#309=MANIFOLD_SOLID_BREP('Body1',#2374);
#310=MANIFOLD_SOLID_BREP('Body1',#2377);
#311=MANIFOLD_SOLID_BREP('Body1',#2378);
#312=MANIFOLD_SOLID_BREP('Body1',#2379);
#313=MANIFOLD_SOLID_BREP('Body1',#2380);
#314=MANIFOLD_SOLID_BREP('Body2',#2381);
#315=MANIFOLD_SOLID_BREP('Body3',#2382);
#316=MANIFOLD_SOLID_BREP('Body4',#2383);
#317=MANIFOLD_SOLID_BREP('Body5',#2384);
#318=MANIFOLD_SOLID_BREP('Body6',#2385);
#319=MANIFOLD_SOLID_BREP('Body7',#2386);
#320=MANIFOLD_SOLID_BREP('Continuous crown cage',#2387);
#321=MANIFOLD_SOLID_BREP('Body1',#2388);
#322=MANIFOLD_SOLID_BREP('Body2',#2389);
#323=MANIFOLD_SOLID_BREP('Body1',#2390);
#324=FACE_BOUND('',#598,.T.);
#325=FACE_BOUND('',#599,.T.);
#326=FACE_BOUND('',#602,.T.);
#327=FACE_BOUND('',#603,.T.);
#328=FACE_BOUND('',#612,.T.);
#329=FACE_BOUND('',#613,.T.);
#330=FACE_BOUND('',#614,.T.);
#331=FACE_BOUND('',#615,.T.);
#332=FACE_BOUND('',#618,.T.);
#333=FACE_BOUND('',#619,.T.);
#334=FACE_BOUND('',#620,.T.);
#335=FACE_BOUND('',#621,.T.);
#336=FACE_BOUND('',#630,.T.);
#337=FACE_BOUND('',#633,.T.);
#338=FACE_BOUND('',#637,.T.);
#339=FACE_BOUND('',#639,.T.);
#340=FACE_BOUND('',#645,.T.);
#341=FACE_BOUND('',#661,.T.);
#342=FACE_BOUND('',#666,.T.);
#343=FACE_BOUND('',#670,.T.);
#344=FACE_BOUND('',#672,.T.);
#345=FACE_BOUND('',#676,.T.);
#346=FACE_BOUND('',#678,.T.);
#347=FACE_BOUND('',#682,.T.);
#348=FACE_BOUND('',#684,.T.);
#349=FACE_BOUND('',#699,.T.);
#350=FACE_BOUND('',#704,.T.);
#351=FACE_BOUND('',#707,.T.);
#352=FACE_BOUND('',#711,.T.);
#353=FACE_BOUND('',#713,.T.);
#354=FACE_BOUND('',#719,.T.);
#355=FACE_BOUND('',#722,.T.);
#356=FACE_BOUND('',#727,.T.);
#357=FACE_BOUND('',#732,.T.);
#358=FACE_BOUND('',#757,.T.);
#359=FACE_BOUND('',#760,.T.);
#360=FACE_BOUND('',#763,.T.);
#361=FACE_BOUND('',#766,.T.);
#362=FACE_BOUND('',#769,.T.);
#363=FACE_BOUND('',#774,.T.);
#364=FACE_BOUND('',#776,.T.);
#365=PLANE('',#2585);
#366=PLANE('',#2589);
#367=PLANE('',#2593);
#368=PLANE('',#2597);
#369=PLANE('',#2598);
#370=PLANE('',#2599);
#371=PLANE('',#2600);
#372=PLANE('',#2601);
#373=PLANE('',#2602);
#374=PLANE('',#2603);
#375=PLANE('',#2617);
#376=PLANE('',#2618);
#377=PLANE('',#2619);
#378=PLANE('',#2620);
#379=PLANE('',#2621);
#380=PLANE('',#2622);
#381=PLANE('',#2627);
#382=PLANE('',#2628);
#383=PLANE('',#2629);
#384=PLANE('',#2630);
#385=PLANE('',#2634);
#386=PLANE('',#2642);
#387=PLANE('',#2643);
#388=PLANE('',#2645);
#389=PLANE('',#2653);
#390=PLANE('',#2661);
#391=PLANE('',#2662);
#392=PLANE('',#2663);
#393=PLANE('',#2664);
#394=PLANE('',#2665);
#395=PLANE('',#2666);
#396=PLANE('',#2667);
#397=PLANE('',#2668);
#398=PLANE('',#2669);
#399=PLANE('',#2674);
#400=PLANE('',#2675);
#401=PLANE('',#2680);
#402=PLANE('',#2683);
#403=PLANE('',#2691);
#404=PLANE('',#2692);
#405=PLANE('',#2700);
#406=PLANE('',#2701);
#407=PLANE('',#2709);
#408=PLANE('',#2710);
#409=PLANE('',#2712);
#410=PLANE('',#2713);
#411=PLANE('',#2714);
#412=PLANE('',#2715);
#413=PLANE('',#2716);
#414=PLANE('',#2717);
#415=PLANE('',#2718);
#416=PLANE('',#2719);
#417=PLANE('',#2720);
#418=PLANE('',#2722);
#419=PLANE('',#2730);
#420=PLANE('',#2772);
#421=PLANE('',#2777);
#422=PLANE('',#2783);
#423=PLANE('',#2784);
#424=PLANE('',#2800);
#425=PLANE('',#2803);
#426=PLANE('',#2815);
#427=PLANE('',#2824);
#428=PLANE('',#2855);
#429=PLANE('',#2860);
#430=PLANE('',#2865);
#431=PLANE('',#2871);
#432=PLANE('',#2876);
#433=PLANE('',#2885);
#434=PLANE('',#2889);
#435=PLANE('',#2890);
#436=PLANE('',#2892);
#437=PLANE('',#2897);
#438=PLANE('',#2900);
#439=PLANE('',#2905);
#440=PLANE('',#2920);
#441=PLANE('',#2921);
#442=FACE_OUTER_BOUND('',#589,.T.);
#443=FACE_OUTER_BOUND('',#590,.T.);
#444=FACE_OUTER_BOUND('',#591,.T.);
#445=FACE_OUTER_BOUND('',#592,.T.);
#446=FACE_OUTER_BOUND('',#593,.T.);
#447=FACE_OUTER_BOUND('',#594,.T.);
#448=FACE_OUTER_BOUND('',#595,.T.);
#449=FACE_OUTER_BOUND('',#596,.T.);
#450=FACE_OUTER_BOUND('',#597,.T.);
#451=FACE_OUTER_BOUND('',#600,.T.);
#452=FACE_OUTER_BOUND('',#601,.T.);
#453=FACE_OUTER_BOUND('',#604,.T.);
#454=FACE_OUTER_BOUND('',#605,.T.);
#455=FACE_OUTER_BOUND('',#606,.T.);
#456=FACE_OUTER_BOUND('',#607,.T.);
#457=FACE_OUTER_BOUND('',#608,.T.);
#458=FACE_OUTER_BOUND('',#609,.T.);
#459=FACE_OUTER_BOUND('',#610,.T.);
#460=FACE_OUTER_BOUND('',#611,.T.);
#461=FACE_OUTER_BOUND('',#616,.T.);
#462=FACE_OUTER_BOUND('',#617,.T.);
#463=FACE_OUTER_BOUND('',#622,.T.);
#464=FACE_OUTER_BOUND('',#623,.T.);
#465=FACE_OUTER_BOUND('',#624,.T.);
#466=FACE_OUTER_BOUND('',#625,.T.);
#467=FACE_OUTER_BOUND('',#626,.T.);
#468=FACE_OUTER_BOUND('',#627,.T.);
#469=FACE_OUTER_BOUND('',#628,.T.);
#470=FACE_OUTER_BOUND('',#629,.T.);
#471=FACE_OUTER_BOUND('',#631,.T.);
#472=FACE_OUTER_BOUND('',#632,.T.);
#473=FACE_OUTER_BOUND('',#634,.T.);
#474=FACE_OUTER_BOUND('',#635,.T.);
#475=FACE_OUTER_BOUND('',#636,.T.);
#476=FACE_OUTER_BOUND('',#638,.T.);
#477=FACE_OUTER_BOUND('',#640,.T.);
#478=FACE_OUTER_BOUND('',#641,.T.);
#479=FACE_OUTER_BOUND('',#642,.T.);
#480=FACE_OUTER_BOUND('',#643,.T.);
#481=FACE_OUTER_BOUND('',#644,.T.);
#482=FACE_OUTER_BOUND('',#646,.T.);
#483=FACE_OUTER_BOUND('',#647,.T.);
#484=FACE_OUTER_BOUND('',#648,.T.);
#485=FACE_OUTER_BOUND('',#649,.T.);
#486=FACE_OUTER_BOUND('',#650,.T.);
#487=FACE_OUTER_BOUND('',#651,.T.);
#488=FACE_OUTER_BOUND('',#652,.T.);
#489=FACE_OUTER_BOUND('',#653,.T.);
#490=FACE_OUTER_BOUND('',#654,.T.);
#491=FACE_OUTER_BOUND('',#655,.T.);
#492=FACE_OUTER_BOUND('',#656,.T.);
#493=FACE_OUTER_BOUND('',#657,.T.);
#494=FACE_OUTER_BOUND('',#658,.T.);
#495=FACE_OUTER_BOUND('',#659,.T.);
#496=FACE_OUTER_BOUND('',#660,.T.);
#497=FACE_OUTER_BOUND('',#662,.T.);
#498=FACE_OUTER_BOUND('',#663,.T.);
#499=FACE_OUTER_BOUND('',#664,.T.);
#500=FACE_OUTER_BOUND('',#665,.T.);
#501=FACE_OUTER_BOUND('',#667,.T.);
#502=FACE_OUTER_BOUND('',#668,.T.);
#503=FACE_OUTER_BOUND('',#669,.T.);
#504=FACE_OUTER_BOUND('',#671,.T.);
#505=FACE_OUTER_BOUND('',#673,.T.);
#506=FACE_OUTER_BOUND('',#674,.T.);
#507=FACE_OUTER_BOUND('',#675,.T.);
#508=FACE_OUTER_BOUND('',#677,.T.);
#509=FACE_OUTER_BOUND('',#679,.T.);
#510=FACE_OUTER_BOUND('',#680,.T.);
#511=FACE_OUTER_BOUND('',#681,.T.);
#512=FACE_OUTER_BOUND('',#683,.T.);
#513=FACE_OUTER_BOUND('',#685,.T.);
#514=FACE_OUTER_BOUND('',#686,.T.);
#515=FACE_OUTER_BOUND('',#687,.T.);
#516=FACE_OUTER_BOUND('',#688,.T.);
#517=FACE_OUTER_BOUND('',#689,.T.);
#518=FACE_OUTER_BOUND('',#690,.T.);
#519=FACE_OUTER_BOUND('',#691,.T.);
#520=FACE_OUTER_BOUND('',#692,.T.);
#521=FACE_OUTER_BOUND('',#693,.T.);
#522=FACE_OUTER_BOUND('',#694,.T.);
#523=FACE_OUTER_BOUND('',#695,.T.);
#524=FACE_OUTER_BOUND('',#696,.T.);
#525=FACE_OUTER_BOUND('',#697,.T.);
#526=FACE_OUTER_BOUND('',#698,.T.);
#527=FACE_OUTER_BOUND('',#700,.T.);
#528=FACE_OUTER_BOUND('',#701,.T.);
#529=FACE_OUTER_BOUND('',#702,.T.);
#530=FACE_OUTER_BOUND('',#703,.T.);
#531=FACE_OUTER_BOUND('',#705,.T.);
#532=FACE_OUTER_BOUND('',#706,.T.);
#533=FACE_OUTER_BOUND('',#708,.T.);
#534=FACE_OUTER_BOUND('',#709,.T.);
#535=FACE_OUTER_BOUND('',#710,.T.);
#536=FACE_OUTER_BOUND('',#712,.T.);
#537=FACE_OUTER_BOUND('',#714,.T.);
#538=FACE_OUTER_BOUND('',#715,.T.);
#539=FACE_OUTER_BOUND('',#716,.T.);
#540=FACE_OUTER_BOUND('',#717,.T.);
#541=FACE_OUTER_BOUND('',#718,.T.);
#542=FACE_OUTER_BOUND('',#720,.T.);
#543=FACE_OUTER_BOUND('',#721,.T.);
#544=FACE_OUTER_BOUND('',#723,.T.);
#545=FACE_OUTER_BOUND('',#724,.T.);
#546=FACE_OUTER_BOUND('',#725,.T.);
#547=FACE_OUTER_BOUND('',#726,.T.);
#548=FACE_OUTER_BOUND('',#728,.T.);
#549=FACE_OUTER_BOUND('',#729,.T.);
#550=FACE_OUTER_BOUND('',#730,.T.);
#551=FACE_OUTER_BOUND('',#731,.T.);
#552=FACE_OUTER_BOUND('',#733,.T.);
#553=FACE_OUTER_BOUND('',#734,.T.);
#554=FACE_OUTER_BOUND('',#735,.T.);
#555=FACE_OUTER_BOUND('',#736,.T.);
#556=FACE_OUTER_BOUND('',#737,.T.);
#557=FACE_OUTER_BOUND('',#738,.T.);
#558=FACE_OUTER_BOUND('',#739,.T.);
#559=FACE_OUTER_BOUND('',#740,.T.);
#560=FACE_OUTER_BOUND('',#741,.T.);
#561=FACE_OUTER_BOUND('',#742,.T.);
#562=FACE_OUTER_BOUND('',#743,.T.);
#563=FACE_OUTER_BOUND('',#744,.T.);
#564=FACE_OUTER_BOUND('',#745,.T.);
#565=FACE_OUTER_BOUND('',#746,.T.);
#566=FACE_OUTER_BOUND('',#747,.T.);
#567=FACE_OUTER_BOUND('',#748,.T.);
#568=FACE_OUTER_BOUND('',#749,.T.);
#569=FACE_OUTER_BOUND('',#750,.T.);
#570=FACE_OUTER_BOUND('',#751,.T.);
#571=FACE_OUTER_BOUND('',#752,.T.);
#572=FACE_OUTER_BOUND('',#753,.T.);
#573=FACE_OUTER_BOUND('',#754,.T.);
#574=FACE_OUTER_BOUND('',#755,.T.);
#575=FACE_OUTER_BOUND('',#756,.T.);
#576=FACE_OUTER_BOUND('',#758,.T.);
#577=FACE_OUTER_BOUND('',#759,.T.);
#578=FACE_OUTER_BOUND('',#761,.T.);
#579=FACE_OUTER_BOUND('',#762,.T.);
#580=FACE_OUTER_BOUND('',#764,.T.);
#581=FACE_OUTER_BOUND('',#765,.T.);
#582=FACE_OUTER_BOUND('',#767,.T.);
#583=FACE_OUTER_BOUND('',#768,.T.);
#584=FACE_OUTER_BOUND('',#770,.T.);
#585=FACE_OUTER_BOUND('',#771,.T.);
#586=FACE_OUTER_BOUND('',#772,.T.);
#587=FACE_OUTER_BOUND('',#773,.T.);
#588=FACE_OUTER_BOUND('',#775,.T.);
#589=EDGE_LOOP('',(#1625,#1626,#1627,#1628));
#590=EDGE_LOOP('',(#1629));
#591=EDGE_LOOP('',(#1630,#1631,#1632,#1633));
#592=EDGE_LOOP('',(#1634));
#593=EDGE_LOOP('',(#1635,#1636,#1637,#1638));
#594=EDGE_LOOP('',(#1639));
#595=EDGE_LOOP('',(#1640,#1641,#1642,#1643));
#596=EDGE_LOOP('',(#1644));
#597=EDGE_LOOP('',(#1645,#1646,#1647,#1648));
#598=EDGE_LOOP('',(#1649));
#599=EDGE_LOOP('',(#1650));
#600=EDGE_LOOP('',(#1651,#1652,#1653,#1654));
#601=EDGE_LOOP('',(#1655,#1656,#1657,#1658));
#602=EDGE_LOOP('',(#1659));
#603=EDGE_LOOP('',(#1660));
#604=EDGE_LOOP('',(#1661,#1662,#1663,#1664));
#605=EDGE_LOOP('',(#1665,#1666,#1667,#1668));
#606=EDGE_LOOP('',(#1669,#1670,#1671,#1672));
#607=EDGE_LOOP('',(#1673,#1674,#1675,#1676));
#608=EDGE_LOOP('',(#1677,#1678,#1679,#1680));
#609=EDGE_LOOP('',(#1681,#1682,#1683,#1684));
#610=EDGE_LOOP('',(#1685,#1686,#1687,#1688));
#611=EDGE_LOOP('',(#1689,#1690,#1691,#1692));
#612=EDGE_LOOP('',(#1693));
#613=EDGE_LOOP('',(#1694));
#614=EDGE_LOOP('',(#1695));
#615=EDGE_LOOP('',(#1696));
#616=EDGE_LOOP('',(#1697,#1698,#1699,#1700));
#617=EDGE_LOOP('',(#1701,#1702,#1703,#1704));
#618=EDGE_LOOP('',(#1705));
#619=EDGE_LOOP('',(#1706));
#620=EDGE_LOOP('',(#1707));
#621=EDGE_LOOP('',(#1708));
#622=EDGE_LOOP('',(#1709,#1710,#1711,#1712));
#623=EDGE_LOOP('',(#1713,#1714,#1715,#1716));
#624=EDGE_LOOP('',(#1717,#1718,#1719,#1720));
#625=EDGE_LOOP('',(#1721,#1722,#1723,#1724));
#626=EDGE_LOOP('',(#1725,#1726,#1727,#1728));
#627=EDGE_LOOP('',(#1729,#1730,#1731,#1732));
#628=EDGE_LOOP('',(#1733,#1734,#1735,#1736));
#629=EDGE_LOOP('',(#1737,#1738,#1739,#1740));
#630=EDGE_LOOP('',(#1741));
#631=EDGE_LOOP('',(#1742,#1743,#1744,#1745));
#632=EDGE_LOOP('',(#1746,#1747,#1748,#1749));
#633=EDGE_LOOP('',(#1750));
#634=EDGE_LOOP('',(#1751,#1752,#1753,#1754));
#635=EDGE_LOOP('',(#1755,#1756,#1757,#1758));
#636=EDGE_LOOP('',(#1759));
#637=EDGE_LOOP('',(#1760));
#638=EDGE_LOOP('',(#1761));
#639=EDGE_LOOP('',(#1762));
#640=EDGE_LOOP('',(#1763));
#641=EDGE_LOOP('',(#1764,#1765,#1766,#1767));
#642=EDGE_LOOP('',(#1768,#1769,#1770,#1771));
#643=EDGE_LOOP('',(#1772,#1773,#1774,#1775));
#644=EDGE_LOOP('',(#1776));
#645=EDGE_LOOP('',(#1777));
#646=EDGE_LOOP('',(#1778,#1779,#1780,#1781));
#647=EDGE_LOOP('',(#1782,#1783,#1784,#1785));
#648=EDGE_LOOP('',(#1786,#1787,#1788,#1789));
#649=EDGE_LOOP('',(#1790));
#650=EDGE_LOOP('',(#1791,#1792,#1793,#1794));
#651=EDGE_LOOP('',(#1795,#1796,#1797,#1798));
#652=EDGE_LOOP('',(#1799,#1800,#1801,#1802));
#653=EDGE_LOOP('',(#1803,#1804,#1805,#1806));
#654=EDGE_LOOP('',(#1807,#1808,#1809,#1810));
#655=EDGE_LOOP('',(#1811,#1812,#1813,#1814));
#656=EDGE_LOOP('',(#1815,#1816,#1817,#1818,#1819,#1820));
#657=EDGE_LOOP('',(#1821,#1822,#1823,#1824,#1825,#1826));
#658=EDGE_LOOP('',(#1827,#1828,#1829,#1830));
#659=EDGE_LOOP('',(#1831));
#660=EDGE_LOOP('',(#1832));
#661=EDGE_LOOP('',(#1833));
#662=EDGE_LOOP('',(#1834,#1835,#1836,#1837));
#663=EDGE_LOOP('',(#1838));
#664=EDGE_LOOP('',(#1839,#1840,#1841,#1842));
#665=EDGE_LOOP('',(#1843));
#666=EDGE_LOOP('',(#1844));
#667=EDGE_LOOP('',(#1845,#1846,#1847,#1848));
#668=EDGE_LOOP('',(#1849,#1850,#1851,#1852));
#669=EDGE_LOOP('',(#1853));
#670=EDGE_LOOP('',(#1854));
#671=EDGE_LOOP('',(#1855));
#672=EDGE_LOOP('',(#1856));
#673=EDGE_LOOP('',(#1857,#1858,#1859,#1860));
#674=EDGE_LOOP('',(#1861,#1862,#1863,#1864));
#675=EDGE_LOOP('',(#1865));
#676=EDGE_LOOP('',(#1866));
#677=EDGE_LOOP('',(#1867));
#678=EDGE_LOOP('',(#1868));
#679=EDGE_LOOP('',(#1869,#1870,#1871,#1872));
#680=EDGE_LOOP('',(#1873,#1874,#1875,#1876));
#681=EDGE_LOOP('',(#1877));
#682=EDGE_LOOP('',(#1878));
#683=EDGE_LOOP('',(#1879));
#684=EDGE_LOOP('',(#1880));
#685=EDGE_LOOP('',(#1881,#1882,#1883,#1884));
#686=EDGE_LOOP('',(#1885,#1886,#1887,#1888));
#687=EDGE_LOOP('',(#1889,#1890,#1891,#1892));
#688=EDGE_LOOP('',(#1893,#1894,#1895,#1896));
#689=EDGE_LOOP('',(#1897,#1898,#1899,#1900));
#690=EDGE_LOOP('',(#1901,#1902,#1903,#1904));
#691=EDGE_LOOP('',(#1905,#1906,#1907,#1908,#1909,#1910));
#692=EDGE_LOOP('',(#1911,#1912,#1913,#1914,#1915,#1916));
#693=EDGE_LOOP('',(#1917));
#694=EDGE_LOOP('',(#1918));
#695=EDGE_LOOP('',(#1919,#1920,#1921,#1922));
#696=EDGE_LOOP('',(#1923,#1924,#1925,#1926));
#697=EDGE_LOOP('',(#1927,#1928,#1929,#1930));
#698=EDGE_LOOP('',(#1931));
#699=EDGE_LOOP('',(#1932));
#700=EDGE_LOOP('',(#1933,#1934,#1935,#1936));
#701=EDGE_LOOP('',(#1937,#1938,#1939,#1940));
#702=EDGE_LOOP('',(#1941,#1942,#1943,#1944));
#703=EDGE_LOOP('',(#1945));
#704=EDGE_LOOP('',(#1946));
#705=EDGE_LOOP('',(#1947,#1948,#1949,#1950));
#706=EDGE_LOOP('',(#1951));
#707=EDGE_LOOP('',(#1952));
#708=EDGE_LOOP('',(#1953,#1954,#1955,#1956));
#709=EDGE_LOOP('',(#1957,#1958,#1959,#1960));
#710=EDGE_LOOP('',(#1961));
#711=EDGE_LOOP('',(#1962));
#712=EDGE_LOOP('',(#1963));
#713=EDGE_LOOP('',(#1964));
#714=EDGE_LOOP('',(#1965,#1966,#1967,#1968,#1969,#1970));
#715=EDGE_LOOP('',(#1971,#1972,#1973,#1974,#1975));
#716=EDGE_LOOP('',(#1976,#1977,#1978,#1979));
#717=EDGE_LOOP('',(#1980,#1981,#1982,#1983));
#718=EDGE_LOOP('',(#1984));
#719=EDGE_LOOP('',(#1985));
#720=EDGE_LOOP('',(#1986,#1987,#1988,#1989,#1990));
#721=EDGE_LOOP('',(#1991));
#722=EDGE_LOOP('',(#1992));
#723=EDGE_LOOP('',(#1993,#1994,#1995,#1996));
#724=EDGE_LOOP('',(#1997,#1998,#1999,#2000,#2001,#2002));
#725=EDGE_LOOP('',(#2003,#2004,#2005,#2006,#2007));
#726=EDGE_LOOP('',(#2008));
#727=EDGE_LOOP('',(#2009));
#728=EDGE_LOOP('',(#2010,#2011,#2012,#2013));
#729=EDGE_LOOP('',(#2014,#2015,#2016,#2017));
#730=EDGE_LOOP('',(#2018,#2019,#2020,#2021));
#731=EDGE_LOOP('',(#2022));
#732=EDGE_LOOP('',(#2023));
#733=EDGE_LOOP('',(#2024,#2025,#2026,#2027,#2028));
#734=EDGE_LOOP('',(#2029,#2030));
#735=EDGE_LOOP('',(#2031,#2032));
#736=EDGE_LOOP('',(#2033,#2034));
#737=EDGE_LOOP('',(#2035,#2036));
#738=EDGE_LOOP('',(#2037,#2038));
#739=EDGE_LOOP('',(#2039,#2040));
#740=EDGE_LOOP('',(#2041,#2042));
#741=EDGE_LOOP('',(#2043,#2044,#2045,#2046));
#742=EDGE_LOOP('',(#2047,#2048,#2049,#2050,#2051,#2052,#2053,#2054,#2055,
#2056,#2057,#2058,#2059,#2060,#2061,#2062,#2063,#2064));
#743=EDGE_LOOP('',(#2065,#2066,#2067,#2068));
#744=EDGE_LOOP('',(#2069,#2070,#2071,#2072));
#745=EDGE_LOOP('',(#2073,#2074,#2075,#2076));
#746=EDGE_LOOP('',(#2077,#2078,#2079,#2080));
#747=EDGE_LOOP('',(#2081,#2082,#2083,#2084,#2085,#2086));
#748=EDGE_LOOP('',(#2087,#2088,#2089,#2090));
#749=EDGE_LOOP('',(#2091,#2092,#2093,#2094));
#750=EDGE_LOOP('',(#2095,#2096,#2097,#2098));
#751=EDGE_LOOP('',(#2099,#2100,#2101,#2102));
#752=EDGE_LOOP('',(#2103,#2104,#2105,#2106));
#753=EDGE_LOOP('',(#2107,#2108,#2109,#2110,#2111,#2112,#2113,#2114,#2115,
#2116,#2117,#2118,#2119,#2120,#2121,#2122,#2123,#2124));
#754=EDGE_LOOP('',(#2125,#2126,#2127,#2128));
#755=EDGE_LOOP('',(#2129,#2130,#2131,#2132));
#756=EDGE_LOOP('',(#2133));
#757=EDGE_LOOP('',(#2134));
#758=EDGE_LOOP('',(#2135,#2136,#2137,#2138));
#759=EDGE_LOOP('',(#2139));
#760=EDGE_LOOP('',(#2140));
#761=EDGE_LOOP('',(#2141,#2142,#2143,#2144));
#762=EDGE_LOOP('',(#2145));
#763=EDGE_LOOP('',(#2146));
#764=EDGE_LOOP('',(#2147,#2148,#2149,#2150));
#765=EDGE_LOOP('',(#2151));
#766=EDGE_LOOP('',(#2152));
#767=EDGE_LOOP('',(#2153,#2154,#2155,#2156));
#768=EDGE_LOOP('',(#2157));
#769=EDGE_LOOP('',(#2158));
#770=EDGE_LOOP('',(#2159,#2160,#2161,#2162));
#771=EDGE_LOOP('',(#2163,#2164,#2165,#2166));
#772=EDGE_LOOP('',(#2167,#2168,#2169,#2170));
#773=EDGE_LOOP('',(#2171));
#774=EDGE_LOOP('',(#2172));
#775=EDGE_LOOP('',(#2173));
#776=EDGE_LOOP('',(#2174));
#777=LINE('',#3768,#900);
#778=LINE('',#3775,#901);
#779=LINE('',#3782,#902);
#780=LINE('',#3789,#903);
#781=LINE('',#3795,#904);
#782=LINE('',#3797,#905);
#783=LINE('',#3799,#906);
#784=LINE('',#3800,#907);
#785=LINE('',#3803,#908);
#786=LINE('',#3805,#909);
#787=LINE('',#3806,#910);
#788=LINE('',#3809,#911);
#789=LINE('',#3811,#912);
#790=LINE('',#3812,#913);
#791=LINE('',#3814,#914);
#792=LINE('',#3815,#915);
#793=LINE('',#3823,#916);
#794=LINE('',#3829,#917);
#795=LINE('',#3835,#918);
#796=LINE('',#3841,#919);
#797=LINE('',#3846,#920);
#798=LINE('',#3848,#921);
#799=LINE('',#3850,#922);
#800=LINE('',#3851,#923);
#801=LINE('',#3854,#924);
#802=LINE('',#3856,#925);
#803=LINE('',#3857,#926);
#804=LINE('',#3860,#927);
#805=LINE('',#3862,#928);
#806=LINE('',#3863,#929);
#807=LINE('',#3865,#930);
#808=LINE('',#3866,#931);
#809=LINE('',#3874,#932);
#810=LINE('',#3879,#933);
#811=LINE('',#3881,#934);
#812=LINE('',#3883,#935);
#813=LINE('',#3884,#936);
#814=LINE('',#3888,#937);
#815=LINE('',#3890,#938);
#816=LINE('',#3892,#939);
#817=LINE('',#3893,#940);
#818=LINE('',#3895,#941);
#819=LINE('',#3896,#942);
#820=LINE('',#3907,#943);
#821=LINE('',#3913,#944);
#822=LINE('',#3924,#945);
#823=LINE('',#3928,#946);
#824=LINE('',#3932,#947);
#825=LINE('',#3939,#948);
#826=LINE('',#3943,#949);
#827=LINE('',#3947,#950);
#828=LINE('',#3952,#951);
#829=LINE('',#3954,#952);
#830=LINE('',#3956,#953);
#831=LINE('',#3957,#954);
#832=LINE('',#3960,#955);
#833=LINE('',#3962,#956);
#834=LINE('',#3963,#957);
#835=LINE('',#3966,#958);
#836=LINE('',#3968,#959);
#837=LINE('',#3969,#960);
#838=LINE('',#3972,#961);
#839=LINE('',#3974,#962);
#840=LINE('',#3975,#963);
#841=LINE('',#3978,#964);
#842=LINE('',#3980,#965);
#843=LINE('',#3981,#966);
#844=LINE('',#3983,#967);
#845=LINE('',#3984,#968);
#846=LINE('',#3992,#969);
#847=LINE('',#4003,#970);
#848=LINE('',#4007,#971);
#849=LINE('',#4015,#972);
#850=LINE('',#4021,#973);
#851=LINE('',#4030,#974);
#852=LINE('',#4036,#975);
#853=LINE('',#4045,#976);
#854=LINE('',#4051,#977);
#855=LINE('',#4059,#978);
#856=LINE('',#4061,#979);
#857=LINE('',#4063,#980);
#858=LINE('',#4064,#981);
#859=LINE('',#4067,#982);
#860=LINE('',#4069,#983);
#861=LINE('',#4070,#984);
#862=LINE('',#4073,#985);
#863=LINE('',#4075,#986);
#864=LINE('',#4076,#987);
#865=LINE('',#4079,#988);
#866=LINE('',#4081,#989);
#867=LINE('',#4082,#990);
#868=LINE('',#4085,#991);
#869=LINE('',#4087,#992);
#870=LINE('',#4088,#993);
#871=LINE('',#4090,#994);
#872=LINE('',#4091,#995);
#873=LINE('',#4103,#996);
#874=LINE('',#4107,#997);
#875=LINE('',#4111,#998);
#876=LINE('',#4118,#999);
#877=LINE('',#4120,#1000);
#878=LINE('',#4159,#1001);
#879=LINE('',#4168,#1002);
#880=LINE('',#4174,#1003);
#881=LINE('',#4179,#1004);
#882=LINE('',#4197,#1005);
#883=LINE('',#4203,#1006);
#884=LINE('',#4207,#1007);
#885=LINE('',#4213,#1008);
#886=LINE('',#4218,#1009);
#887=LINE('',#4233,#1010);
#888=LINE('',#4242,#1011);
#889=LINE('',#4246,#1012);
#890=LINE('',#4250,#1013);
#891=LINE('',#4253,#1014);
#892=LINE('',#4389,#1015);
#893=LINE('',#4642,#1016);
#894=LINE('',#4684,#1017);
#895=LINE('',#4689,#1018);
#896=LINE('',#4698,#1019);
#897=LINE('',#4703,#1020);
#898=LINE('',#4714,#1021);
#899=LINE('',#4720,#1022);
#900=VECTOR('',#2942,0.34);
#901=VECTOR('',#2951,0.34);
#902=VECTOR('',#2960,0.34);
#903=VECTOR('',#2969,0.34);
#904=VECTOR('',#2976,1.);
#905=VECTOR('',#2977,1.);
#906=VECTOR('',#2978,1.);
#907=VECTOR('',#2979,1.);
#908=VECTOR('',#2982,1.);
#909=VECTOR('',#2983,1.);
#910=VECTOR('',#2984,1.);
#911=VECTOR('',#2987,1.);
#912=VECTOR('',#2988,1.);
#913=VECTOR('',#2989,1.);
#914=VECTOR('',#2992,1.);
#915=VECTOR('',#2993,1.);
#916=VECTOR('',#3004,0.425);
#917=VECTOR('',#3011,0.425);
#918=VECTOR('',#3018,0.6);
#919=VECTOR('',#3025,0.6);
#920=VECTOR('',#3030,1.);
#921=VECTOR('',#3031,1.);
#922=VECTOR('',#3032,1.);
#923=VECTOR('',#3033,1.);
#924=VECTOR('',#3036,1.);
#925=VECTOR('',#3037,1.);
#926=VECTOR('',#3038,1.);
#927=VECTOR('',#3041,1.);
#928=VECTOR('',#3042,1.);
#929=VECTOR('',#3043,1.);
#930=VECTOR('',#3046,1.);
#931=VECTOR('',#3047,1.);
#932=VECTOR('',#3058,0.510000000000002);
#933=VECTOR('',#3063,1.);
#934=VECTOR('',#3064,1.);
#935=VECTOR('',#3065,1.);
#936=VECTOR('',#3066,1.);
#937=VECTOR('',#3069,1.);
#938=VECTOR('',#3070,1.);
#939=VECTOR('',#3071,1.);
#940=VECTOR('',#3072,1.);
#941=VECTOR('',#3075,1.);
#942=VECTOR('',#3076,1.);
#943=VECTOR('',#3093,0.42);
#944=VECTOR('',#3100,0.8);
#945=VECTOR('',#3117,0.625);
#946=VECTOR('',#3122,0.65);
#947=VECTOR('',#3127,0.635);
#948=VECTOR('',#3136,0.41);
#949=VECTOR('',#3141,0.4);
#950=VECTOR('',#3146,0.36);
#951=VECTOR('',#3151,1.);
#952=VECTOR('',#3152,1.);
#953=VECTOR('',#3153,1.);
#954=VECTOR('',#3154,1.);
#955=VECTOR('',#3157,1.);
#956=VECTOR('',#3158,1.);
#957=VECTOR('',#3159,1.);
#958=VECTOR('',#3162,1.);
#959=VECTOR('',#3163,1.);
#960=VECTOR('',#3164,1.);
#961=VECTOR('',#3167,1.);
#962=VECTOR('',#3168,1.);
#963=VECTOR('',#3169,1.);
#964=VECTOR('',#3172,1.);
#965=VECTOR('',#3173,1.);
#966=VECTOR('',#3174,1.);
#967=VECTOR('',#3177,1.);
#968=VECTOR('',#3178,1.);
#969=VECTOR('',#3189,0.165);
#970=VECTOR('',#3204,1.);
#971=VECTOR('',#3209,0.6);
#972=VECTOR('',#3220,0.605);
#973=VECTOR('',#3227,0.8);
#974=VECTOR('',#3240,0.605);
#975=VECTOR('',#3247,0.8);
#976=VECTOR('',#3260,0.225);
#977=VECTOR('',#3267,0.8);
#978=VECTOR('',#3278,1.);
#979=VECTOR('',#3279,1.);
#980=VECTOR('',#3280,1.);
#981=VECTOR('',#3281,1.);
#982=VECTOR('',#3284,1.);
#983=VECTOR('',#3285,1.);
#984=VECTOR('',#3286,1.);
#985=VECTOR('',#3289,1.);
#986=VECTOR('',#3290,1.);
#987=VECTOR('',#3291,1.);
#988=VECTOR('',#3294,1.);
#989=VECTOR('',#3295,1.);
#990=VECTOR('',#3296,1.);
#991=VECTOR('',#3299,1.);
#992=VECTOR('',#3300,1.);
#993=VECTOR('',#3301,1.);
#994=VECTOR('',#3304,1.);
#995=VECTOR('',#3305,1.);
#996=VECTOR('',#3322,0.325);
#997=VECTOR('',#3327,0.35);
#998=VECTOR('',#3332,0.335);
#999=VECTOR('',#3341,0.21);
#1000=VECTOR('',#3344,0.2);
#1001=VECTOR('',#3417,1.6);
#1002=VECTOR('',#3428,1.6);
#1003=VECTOR('',#3437,0.62);
#1004=VECTOR('',#3442,3.75);
#1005=VECTOR('',#3467,1.070235);
#1006=VECTOR('',#3474,0.6);
#1007=VECTOR('',#3479,0.63);
#1008=VECTOR('',#3488,1.070235);
#1009=VECTOR('',#3495,0.63);
#1010=VECTOR('',#3514,1.129765);
#1011=VECTOR('',#3525,1.57);
#1012=VECTOR('',#3530,1.6);
#1013=VECTOR('',#3535,1.57);
#1014=VECTOR('',#3540,1.129765);
#1015=VECTOR('',#3587,1.123812);
#1016=VECTOR('',#3656,1.076188);
#1017=VECTOR('',#3685,1.119765);
#1018=VECTOR('',#3692,1.085235);
#1019=VECTOR('',#3703,1.119765);
#1020=VECTOR('',#3710,1.085235);
#1021=VECTOR('',#3727,1.2);
#1022=VECTOR('',#3734,1.6);
#1023=CIRCLE('',#2583,0.34);
#1024=CIRCLE('',#2584,0.34);
#1025=CIRCLE('',#2587,0.34);
#1026=CIRCLE('',#2588,0.34);
#1027=CIRCLE('',#2591,0.34);
#1028=CIRCLE('',#2592,0.34);
#1029=CIRCLE('',#2595,0.34);
#1030=CIRCLE('',#2596,0.34);
#1031=CIRCLE('',#2606,0.425);
#1032=CIRCLE('',#2607,0.425);
#1033=CIRCLE('',#2609,0.425);
#1034=CIRCLE('',#2610,0.425);
#1035=CIRCLE('',#2612,0.6);
#1036=CIRCLE('',#2613,0.6);
#1037=CIRCLE('',#2615,0.6);
#1038=CIRCLE('',#2616,0.6);
#1039=CIRCLE('',#2625,0.510000000000002);
#1040=CIRCLE('',#2626,0.510000000000002);
#1041=CIRCLE('',#2631,2.);
#1042=CIRCLE('',#2633,2.);
#1043=CIRCLE('',#2637,0.42);
#1044=CIRCLE('',#2638,0.42);
#1045=CIRCLE('',#2640,0.8);
#1046=CIRCLE('',#2641,0.8);
#1047=CIRCLE('',#2646,0.6);
#1048=CIRCLE('',#2648,0.65);
#1049=CIRCLE('',#2650,0.65);
#1050=CIRCLE('',#2652,0.62);
#1051=CIRCLE('',#2654,0.42);
#1052=CIRCLE('',#2656,0.3933);
#1053=CIRCLE('',#2658,0.3933);
#1054=CIRCLE('',#2660,0.32);
#1055=CIRCLE('',#2672,0.165);
#1056=CIRCLE('',#2673,0.165);
#1057=CIRCLE('',#2676,1.);
#1058=CIRCLE('',#2677,0.6);
#1059=CIRCLE('',#2679,1.);
#1060=CIRCLE('',#2682,0.6);
#1061=CIRCLE('',#2686,0.605);
#1062=CIRCLE('',#2687,0.605);
#1063=CIRCLE('',#2689,0.8);
#1064=CIRCLE('',#2690,0.8);
#1065=CIRCLE('',#2695,0.605);
#1066=CIRCLE('',#2696,0.605);
#1067=CIRCLE('',#2698,0.8);
#1068=CIRCLE('',#2699,0.8);
#1069=CIRCLE('',#2704,0.225);
#1070=CIRCLE('',#2705,0.225);
#1071=CIRCLE('',#2707,0.8);
#1072=CIRCLE('',#2708,0.8);
#1073=CIRCLE('',#2721,0.1954);
#1074=CIRCLE('',#2723,0.3);
#1075=CIRCLE('',#2725,0.35);
#1076=CIRCLE('',#2727,0.35);
#1077=CIRCLE('',#2729,0.32);
#1078=CIRCLE('',#2731,0.22);
#1079=CIRCLE('',#2733,0.1954);
#1080=CIRCLE('',#2770,1.6);
#1081=CIRCLE('',#2771,1.6);
#1082=CIRCLE('',#2773,0.62);
#1083=CIRCLE('',#2775,1.6);
#1084=CIRCLE('',#2776,1.6);
#1085=CIRCLE('',#2778,0.62);
#1086=CIRCLE('',#2781,3.75);
#1087=CIRCLE('',#2782,3.75);
#1088=CIRCLE('',#2788,1.070235);
#1089=CIRCLE('',#2789,1.070235);
#1090=CIRCLE('',#2790,0.309556);
#1091=CIRCLE('',#2791,1.070235);
#1092=CIRCLE('',#2792,1.070235);
#1093=CIRCLE('',#2794,1.070235);
#1094=CIRCLE('',#2796,0.6);
#1095=CIRCLE('',#2797,0.6);
#1096=CIRCLE('',#2799,0.66);
#1097=CIRCLE('',#2802,1.070235);
#1098=CIRCLE('',#2804,0.66);
#1099=CIRCLE('',#2808,1.129765);
#1100=CIRCLE('',#2809,1.129765);
#1101=CIRCLE('',#2810,0.309556);
#1102=CIRCLE('',#2811,1.129765);
#1103=CIRCLE('',#2812,1.129765);
#1104=CIRCLE('',#2814,1.129765);
#1105=CIRCLE('',#2816,1.54);
#1106=CIRCLE('',#2817,1.129765);
#1107=CIRCLE('',#2819,1.6);
#1108=CIRCLE('',#2821,1.6);
#1109=CIRCLE('',#2823,1.54);
#1110=CIRCLE('',#2828,0.29765);
#1111=CIRCLE('',#2830,0.29765);
#1112=CIRCLE('',#2832,0.29765);
#1113=CIRCLE('',#2834,0.29765);
#1114=CIRCLE('',#2836,0.29765);
#1115=CIRCLE('',#2838,0.29765);
#1116=CIRCLE('',#2840,0.29765);
#1117=CIRCLE('',#2843,0.303778037777585);
#1118=CIRCLE('',#2844,0.303778037777585);
#1119=CIRCLE('',#2846,1.123812);
#1120=CIRCLE('',#2847,1.123812);
#1121=CIRCLE('',#2848,1.123812);
#1122=CIRCLE('',#2849,1.123812);
#1123=CIRCLE('',#2850,1.123812);
#1124=CIRCLE('',#2851,1.123812);
#1125=CIRCLE('',#2852,1.123812);
#1126=CIRCLE('',#2853,1.123812);
#1127=CIRCLE('',#2854,1.123812);
#1128=CIRCLE('',#2856,1.076188);
#1129=CIRCLE('',#2857,0.303778037777585);
#1130=CIRCLE('',#2859,0.303778037777585);
#1131=CIRCLE('',#2861,1.076188);
#1132=CIRCLE('',#2862,0.303778037777585);
#1133=CIRCLE('',#2864,0.303778037777585);
#1134=CIRCLE('',#2866,1.076188);
#1135=CIRCLE('',#2867,1.076188);
#1136=CIRCLE('',#2868,0.303778037777585);
#1137=CIRCLE('',#2870,0.303778037777585);
#1138=CIRCLE('',#2872,1.076188);
#1139=CIRCLE('',#2873,0.303778037777585);
#1140=CIRCLE('',#2875,0.303778037777585);
#1141=CIRCLE('',#2877,1.076188);
#1142=CIRCLE('',#2878,0.303778037777585);
#1143=CIRCLE('',#2880,0.303778037777585);
#1144=CIRCLE('',#2882,1.076188);
#1145=CIRCLE('',#2883,1.076188);
#1146=CIRCLE('',#2884,1.076188);
#1147=CIRCLE('',#2886,0.303778037777585);
#1148=CIRCLE('',#2888,0.303778037777585);
#1149=CIRCLE('',#2893,1.119765);
#1150=CIRCLE('',#2894,1.085235);
#1151=CIRCLE('',#2896,1.119765);
#1152=CIRCLE('',#2898,1.085235);
#1153=CIRCLE('',#2901,1.119765);
#1154=CIRCLE('',#2902,1.085235);
#1155=CIRCLE('',#2904,1.119765);
#1156=CIRCLE('',#2906,1.085235);
#1157=CIRCLE('',#2915,1.2);
#1158=CIRCLE('',#2916,1.2);
#1159=CIRCLE('',#2918,1.6);
#1160=CIRCLE('',#2919,1.6);
#1161=VERTEX_POINT('',#3765);
#1162=VERTEX_POINT('',#3767);
#1163=VERTEX_POINT('',#3772);
#1164=VERTEX_POINT('',#3774);
#1165=VERTEX_POINT('',#3779);
#1166=VERTEX_POINT('',#3781);
#1167=VERTEX_POINT('',#3786);
#1168=VERTEX_POINT('',#3788);
#1169=VERTEX_POINT('',#3793);
#1170=VERTEX_POINT('',#3794);
#1171=VERTEX_POINT('',#3796);
#1172=VERTEX_POINT('',#3798);
#1173=VERTEX_POINT('',#3802);
#1174=VERTEX_POINT('',#3804);
#1175=VERTEX_POINT('',#3808);
#1176=VERTEX_POINT('',#3810);
#1177=VERTEX_POINT('',#3820);
#1178=VERTEX_POINT('',#3822);
#1179=VERTEX_POINT('',#3826);
#1180=VERTEX_POINT('',#3828);
#1181=VERTEX_POINT('',#3832);
#1182=VERTEX_POINT('',#3834);
#1183=VERTEX_POINT('',#3838);
#1184=VERTEX_POINT('',#3840);
#1185=VERTEX_POINT('',#3844);
#1186=VERTEX_POINT('',#3845);
#1187=VERTEX_POINT('',#3847);
#1188=VERTEX_POINT('',#3849);
#1189=VERTEX_POINT('',#3853);
#1190=VERTEX_POINT('',#3855);
#1191=VERTEX_POINT('',#3859);
#1192=VERTEX_POINT('',#3861);
#1193=VERTEX_POINT('',#3871);
#1194=VERTEX_POINT('',#3873);
#1195=VERTEX_POINT('',#3877);
#1196=VERTEX_POINT('',#3878);
#1197=VERTEX_POINT('',#3880);
#1198=VERTEX_POINT('',#3882);
#1199=VERTEX_POINT('',#3886);
#1200=VERTEX_POINT('',#3887);
#1201=VERTEX_POINT('',#3889);
#1202=VERTEX_POINT('',#3891);
#1203=VERTEX_POINT('',#3904);
#1204=VERTEX_POINT('',#3906);
#1205=VERTEX_POINT('',#3910);
#1206=VERTEX_POINT('',#3912);
#1207=VERTEX_POINT('',#3919);
#1208=VERTEX_POINT('',#3922);
#1209=VERTEX_POINT('',#3926);
#1210=VERTEX_POINT('',#3930);
#1211=VERTEX_POINT('',#3934);
#1212=VERTEX_POINT('',#3937);
#1213=VERTEX_POINT('',#3941);
#1214=VERTEX_POINT('',#3945);
#1215=VERTEX_POINT('',#3950);
#1216=VERTEX_POINT('',#3951);
#1217=VERTEX_POINT('',#3953);
#1218=VERTEX_POINT('',#3955);
#1219=VERTEX_POINT('',#3959);
#1220=VERTEX_POINT('',#3961);
#1221=VERTEX_POINT('',#3965);
#1222=VERTEX_POINT('',#3967);
#1223=VERTEX_POINT('',#3971);
#1224=VERTEX_POINT('',#3973);
#1225=VERTEX_POINT('',#3977);
#1226=VERTEX_POINT('',#3979);
#1227=VERTEX_POINT('',#3989);
#1228=VERTEX_POINT('',#3991);
#1229=VERTEX_POINT('',#3996);
#1230=VERTEX_POINT('',#3998);
#1231=VERTEX_POINT('',#4001);
#1232=VERTEX_POINT('',#4006);
#1233=VERTEX_POINT('',#4012);
#1234=VERTEX_POINT('',#4014);
#1235=VERTEX_POINT('',#4018);
#1236=VERTEX_POINT('',#4020);
#1237=VERTEX_POINT('',#4027);
#1238=VERTEX_POINT('',#4029);
#1239=VERTEX_POINT('',#4033);
#1240=VERTEX_POINT('',#4035);
#1241=VERTEX_POINT('',#4042);
#1242=VERTEX_POINT('',#4044);
#1243=VERTEX_POINT('',#4048);
#1244=VERTEX_POINT('',#4050);
#1245=VERTEX_POINT('',#4057);
#1246=VERTEX_POINT('',#4058);
#1247=VERTEX_POINT('',#4060);
#1248=VERTEX_POINT('',#4062);
#1249=VERTEX_POINT('',#4066);
#1250=VERTEX_POINT('',#4068);
#1251=VERTEX_POINT('',#4072);
#1252=VERTEX_POINT('',#4074);
#1253=VERTEX_POINT('',#4078);
#1254=VERTEX_POINT('',#4080);
#1255=VERTEX_POINT('',#4084);
#1256=VERTEX_POINT('',#4086);
#1257=VERTEX_POINT('',#4095);
#1258=VERTEX_POINT('',#4098);
#1259=VERTEX_POINT('',#4101);
#1260=VERTEX_POINT('',#4105);
#1261=VERTEX_POINT('',#4109);
#1262=VERTEX_POINT('',#4113);
#1263=VERTEX_POINT('',#4116);
#1264=VERTEX_POINT('',#4156);
#1265=VERTEX_POINT('',#4158);
#1266=VERTEX_POINT('',#4162);
#1267=VERTEX_POINT('',#4165);
#1268=VERTEX_POINT('',#4167);
#1269=VERTEX_POINT('',#4171);
#1270=VERTEX_POINT('',#4176);
#1271=VERTEX_POINT('',#4178);
#1272=VERTEX_POINT('',#4186);
#1273=VERTEX_POINT('',#4187);
#1274=VERTEX_POINT('',#4190);
#1275=VERTEX_POINT('',#4192);
#1276=VERTEX_POINT('',#4196);
#1277=VERTEX_POINT('',#4200);
#1278=VERTEX_POINT('',#4202);
#1279=VERTEX_POINT('',#4206);
#1280=VERTEX_POINT('',#4211);
#1281=VERTEX_POINT('',#4215);
#1282=VERTEX_POINT('',#4221);
#1283=VERTEX_POINT('',#4222);
#1284=VERTEX_POINT('',#4225);
#1285=VERTEX_POINT('',#4227);
#1286=VERTEX_POINT('',#4231);
#1287=VERTEX_POINT('',#4235);
#1288=VERTEX_POINT('',#4237);
#1289=VERTEX_POINT('',#4240);
#1290=VERTEX_POINT('',#4244);
#1291=VERTEX_POINT('',#4248);
#1292=VERTEX_POINT('',#4256);
#1293=VERTEX_POINT('',#4257);
#1294=VERTEX_POINT('',#4260);
#1295=VERTEX_POINT('',#4261);
#1296=VERTEX_POINT('',#4264);
#1297=VERTEX_POINT('',#4265);
#1298=VERTEX_POINT('',#4268);
#1299=VERTEX_POINT('',#4269);
#1300=VERTEX_POINT('',#4272);
#1301=VERTEX_POINT('',#4273);
#1302=VERTEX_POINT('',#4276);
#1303=VERTEX_POINT('',#4277);
#1304=VERTEX_POINT('',#4280);
#1305=VERTEX_POINT('',#4281);
#1306=VERTEX_POINT('',#4285);
#1307=VERTEX_POINT('',#4286);
#1308=VERTEX_POINT('',#4309);
#1309=VERTEX_POINT('',#4311);
#1310=VERTEX_POINT('',#4336);
#1311=VERTEX_POINT('',#4338);
#1312=VERTEX_POINT('',#4361);
#1313=VERTEX_POINT('',#4363);
#1314=VERTEX_POINT('',#4386);
#1315=VERTEX_POINT('',#4388);
#1316=VERTEX_POINT('',#4391);
#1317=VERTEX_POINT('',#4393);
#1318=VERTEX_POINT('',#4416);
#1319=VERTEX_POINT('',#4418);
#1320=VERTEX_POINT('',#4441);
#1321=VERTEX_POINT('',#4443);
#1322=VERTEX_POINT('',#4466);
#1323=VERTEX_POINT('',#4468);
#1324=VERTEX_POINT('',#4493);
#1325=VERTEX_POINT('',#4497);
#1326=VERTEX_POINT('',#4522);
#1327=VERTEX_POINT('',#4526);
#1328=VERTEX_POINT('',#4551);
#1329=VERTEX_POINT('',#4553);
#1330=VERTEX_POINT('',#4557);
#1331=VERTEX_POINT('',#4582);
#1332=VERTEX_POINT('',#4586);
#1333=VERTEX_POINT('',#4611);
#1334=VERTEX_POINT('',#4615);
#1335=VERTEX_POINT('',#4640);
#1336=VERTEX_POINT('',#4643);
#1337=VERTEX_POINT('',#4645);
#1338=VERTEX_POINT('',#4677);
#1339=VERTEX_POINT('',#4679);
#1340=VERTEX_POINT('',#4682);
#1341=VERTEX_POINT('',#4686);
#1342=VERTEX_POINT('',#4691);
#1343=VERTEX_POINT('',#4693);
#1344=VERTEX_POINT('',#4696);
#1345=VERTEX_POINT('',#4700);
#1346=VERTEX_POINT('',#4711);
#1347=VERTEX_POINT('',#4713);
#1348=VERTEX_POINT('',#4717);
#1349=VERTEX_POINT('',#4719);
#1350=EDGE_CURVE('',#1161,#1161,#1023,.T.);
#1351=EDGE_CURVE('',#1161,#1162,#777,.T.);
#1352=EDGE_CURVE('',#1162,#1162,#1024,.T.);
#1353=EDGE_CURVE('',#1163,#1163,#1025,.T.);
#1354=EDGE_CURVE('',#1163,#1164,#778,.T.);
#1355=EDGE_CURVE('',#1164,#1164,#1026,.T.);
#1356=EDGE_CURVE('',#1165,#1165,#1027,.T.);
#1357=EDGE_CURVE('',#1165,#1166,#779,.T.);
#1358=EDGE_CURVE('',#1166,#1166,#1028,.T.);
#1359=EDGE_CURVE('',#1167,#1167,#1029,.T.);
#1360=EDGE_CURVE('',#1167,#1168,#780,.T.);
#1361=EDGE_CURVE('',#1168,#1168,#1030,.T.);
#1362=EDGE_CURVE('',#1169,#1170,#781,.T.);
#1363=EDGE_CURVE('',#1170,#1171,#782,.T.);
#1364=EDGE_CURVE('',#1172,#1171,#783,.T.);
#1365=EDGE_CURVE('',#1169,#1172,#784,.T.);
#1366=EDGE_CURVE('',#1173,#1169,#785,.T.);
#1367=EDGE_CURVE('',#1174,#1172,#786,.T.);
#1368=EDGE_CURVE('',#1173,#1174,#787,.T.);
#1369=EDGE_CURVE('',#1175,#1173,#788,.T.);
#1370=EDGE_CURVE('',#1176,#1174,#789,.T.);
#1371=EDGE_CURVE('',#1175,#1176,#790,.T.);
#1372=EDGE_CURVE('',#1170,#1175,#791,.T.);
#1373=EDGE_CURVE('',#1171,#1176,#792,.T.);
#1374=EDGE_CURVE('',#1177,#1177,#1031,.T.);
#1375=EDGE_CURVE('',#1177,#1178,#793,.T.);
#1376=EDGE_CURVE('',#1178,#1178,#1032,.T.);
#1377=EDGE_CURVE('',#1179,#1179,#1033,.T.);
#1378=EDGE_CURVE('',#1179,#1180,#794,.T.);
#1379=EDGE_CURVE('',#1180,#1180,#1034,.T.);
#1380=EDGE_CURVE('',#1181,#1181,#1035,.T.);
#1381=EDGE_CURVE('',#1181,#1182,#795,.T.);
#1382=EDGE_CURVE('',#1182,#1182,#1036,.T.);
#1383=EDGE_CURVE('',#1183,#1183,#1037,.T.);
#1384=EDGE_CURVE('',#1183,#1184,#796,.T.);
#1385=EDGE_CURVE('',#1184,#1184,#1038,.T.);
#1386=EDGE_CURVE('',#1185,#1186,#797,.T.);
#1387=EDGE_CURVE('',#1186,#1187,#798,.T.);
#1388=EDGE_CURVE('',#1188,#1187,#799,.T.);
#1389=EDGE_CURVE('',#1185,#1188,#800,.T.);
#1390=EDGE_CURVE('',#1189,#1185,#801,.T.);
#1391=EDGE_CURVE('',#1190,#1188,#802,.T.);
#1392=EDGE_CURVE('',#1189,#1190,#803,.T.);
#1393=EDGE_CURVE('',#1191,#1189,#804,.T.);
#1394=EDGE_CURVE('',#1192,#1190,#805,.T.);
#1395=EDGE_CURVE('',#1191,#1192,#806,.T.);
#1396=EDGE_CURVE('',#1186,#1191,#807,.T.);
#1397=EDGE_CURVE('',#1187,#1192,#808,.T.);
#1398=EDGE_CURVE('',#1193,#1193,#1039,.T.);
#1399=EDGE_CURVE('',#1193,#1194,#809,.T.);
#1400=EDGE_CURVE('',#1194,#1194,#1040,.T.);
#1401=EDGE_CURVE('',#1195,#1196,#810,.T.);
#1402=EDGE_CURVE('',#1195,#1197,#811,.T.);
#1403=EDGE_CURVE('',#1198,#1197,#812,.T.);
#1404=EDGE_CURVE('',#1196,#1198,#813,.T.);
#1405=EDGE_CURVE('',#1199,#1200,#814,.T.);
#1406=EDGE_CURVE('',#1201,#1199,#815,.T.);
#1407=EDGE_CURVE('',#1202,#1201,#816,.T.);
#1408=EDGE_CURVE('',#1200,#1202,#817,.T.);
#1409=EDGE_CURVE('',#1197,#1202,#818,.T.);
#1410=EDGE_CURVE('',#1200,#1195,#819,.T.);
#1411=EDGE_CURVE('',#1201,#1198,#1041,.T.);
#1412=EDGE_CURVE('',#1199,#1196,#1042,.T.);
#1413=EDGE_CURVE('',#1203,#1203,#1043,.T.);
#1414=EDGE_CURVE('',#1203,#1204,#820,.T.);
#1415=EDGE_CURVE('',#1204,#1204,#1044,.T.);
#1416=EDGE_CURVE('',#1205,#1205,#1045,.T.);
#1417=EDGE_CURVE('',#1205,#1206,#821,.T.);
#1418=EDGE_CURVE('',#1206,#1206,#1046,.T.);
#1419=EDGE_CURVE('',#1207,#1207,#1047,.T.);
#1420=EDGE_CURVE('',#1208,#1208,#1048,.T.);
#1421=EDGE_CURVE('',#1208,#1207,#822,.T.);
#1422=EDGE_CURVE('',#1209,#1209,#1049,.T.);
#1423=EDGE_CURVE('',#1209,#1208,#823,.T.);
#1424=EDGE_CURVE('',#1210,#1210,#1050,.T.);
#1425=EDGE_CURVE('',#1210,#1209,#824,.T.);
#1426=EDGE_CURVE('',#1211,#1211,#1051,.T.);
#1427=EDGE_CURVE('',#1212,#1212,#1052,.F.);
#1428=EDGE_CURVE('',#1212,#1211,#825,.T.);
#1429=EDGE_CURVE('',#1213,#1213,#1053,.F.);
#1430=EDGE_CURVE('',#1213,#1212,#826,.T.);
#1431=EDGE_CURVE('',#1214,#1214,#1054,.T.);
#1432=EDGE_CURVE('',#1214,#1213,#827,.T.);
#1433=EDGE_CURVE('',#1215,#1216,#828,.T.);
#1434=EDGE_CURVE('',#1216,#1217,#829,.T.);
#1435=EDGE_CURVE('',#1217,#1218,#830,.T.);
#1436=EDGE_CURVE('',#1215,#1218,#831,.T.);
#1437=EDGE_CURVE('',#1216,#1219,#832,.T.);
#1438=EDGE_CURVE('',#1219,#1220,#833,.T.);
#1439=EDGE_CURVE('',#1220,#1217,#834,.T.);
#1440=EDGE_CURVE('',#1219,#1221,#835,.T.);
#1441=EDGE_CURVE('',#1221,#1222,#836,.T.);
#1442=EDGE_CURVE('',#1222,#1220,#837,.T.);
#1443=EDGE_CURVE('',#1221,#1223,#838,.T.);
#1444=EDGE_CURVE('',#1223,#1224,#839,.T.);
#1445=EDGE_CURVE('',#1224,#1222,#840,.T.);
#1446=EDGE_CURVE('',#1223,#1225,#841,.T.);
#1447=EDGE_CURVE('',#1225,#1226,#842,.T.);
#1448=EDGE_CURVE('',#1226,#1224,#843,.T.);
#1449=EDGE_CURVE('',#1225,#1215,#844,.T.);
#1450=EDGE_CURVE('',#1218,#1226,#845,.T.);
#1451=EDGE_CURVE('',#1227,#1227,#1055,.T.);
#1452=EDGE_CURVE('',#1227,#1228,#846,.T.);
#1453=EDGE_CURVE('',#1228,#1228,#1056,.T.);
#1454=EDGE_CURVE('',#1229,#1229,#1057,.T.);
#1455=EDGE_CURVE('',#1230,#1230,#1058,.T.);
#1456=EDGE_CURVE('',#1231,#1231,#1059,.T.);
#1457=EDGE_CURVE('',#1231,#1229,#847,.T.);
#1458=EDGE_CURVE('',#1230,#1232,#848,.T.);
#1459=EDGE_CURVE('',#1232,#1232,#1060,.T.);
#1460=EDGE_CURVE('',#1233,#1233,#1061,.T.);
#1461=EDGE_CURVE('',#1233,#1234,#849,.T.);
#1462=EDGE_CURVE('',#1234,#1234,#1062,.T.);
#1463=EDGE_CURVE('',#1235,#1235,#1063,.T.);
#1464=EDGE_CURVE('',#1235,#1236,#850,.T.);
#1465=EDGE_CURVE('',#1236,#1236,#1064,.T.);
#1466=EDGE_CURVE('',#1237,#1237,#1065,.T.);
#1467=EDGE_CURVE('',#1237,#1238,#851,.T.);
#1468=EDGE_CURVE('',#1238,#1238,#1066,.T.);
#1469=EDGE_CURVE('',#1239,#1239,#1067,.T.);
#1470=EDGE_CURVE('',#1239,#1240,#852,.T.);
#1471=EDGE_CURVE('',#1240,#1240,#1068,.T.);
#1472=EDGE_CURVE('',#1241,#1241,#1069,.T.);
#1473=EDGE_CURVE('',#1241,#1242,#853,.T.);
#1474=EDGE_CURVE('',#1242,#1242,#1070,.T.);
#1475=EDGE_CURVE('',#1243,#1243,#1071,.T.);
#1476=EDGE_CURVE('',#1243,#1244,#854,.T.);
#1477=EDGE_CURVE('',#1244,#1244,#1072,.T.);
#1478=EDGE_CURVE('',#1245,#1246,#855,.T.);
#1479=EDGE_CURVE('',#1246,#1247,#856,.T.);
#1480=EDGE_CURVE('',#1247,#1248,#857,.T.);
#1481=EDGE_CURVE('',#1245,#1248,#858,.T.);
#1482=EDGE_CURVE('',#1246,#1249,#859,.T.);
#1483=EDGE_CURVE('',#1249,#1250,#860,.T.);
#1484=EDGE_CURVE('',#1250,#1247,#861,.T.);
#1485=EDGE_CURVE('',#1249,#1251,#862,.T.);
#1486=EDGE_CURVE('',#1251,#1252,#863,.T.);
#1487=EDGE_CURVE('',#1252,#1250,#864,.T.);
#1488=EDGE_CURVE('',#1251,#1253,#865,.T.);
#1489=EDGE_CURVE('',#1253,#1254,#866,.T.);
#1490=EDGE_CURVE('',#1254,#1252,#867,.T.);
#1491=EDGE_CURVE('',#1253,#1255,#868,.T.);
#1492=EDGE_CURVE('',#1255,#1256,#869,.T.);
#1493=EDGE_CURVE('',#1256,#1254,#870,.T.);
#1494=EDGE_CURVE('',#1255,#1245,#871,.T.);
#1495=EDGE_CURVE('',#1248,#1256,#872,.T.);
#1496=EDGE_CURVE('',#1257,#1257,#1073,.T.);
#1497=EDGE_CURVE('',#1258,#1258,#1074,.T.);
#1498=EDGE_CURVE('',#1259,#1259,#1075,.T.);
#1499=EDGE_CURVE('',#1259,#1258,#873,.T.);
#1500=EDGE_CURVE('',#1260,#1260,#1076,.T.);
#1501=EDGE_CURVE('',#1260,#1259,#874,.T.);
#1502=EDGE_CURVE('',#1261,#1261,#1077,.T.);
#1503=EDGE_CURVE('',#1261,#1260,#875,.T.);
#1504=EDGE_CURVE('',#1262,#1262,#1078,.T.);
#1505=EDGE_CURVE('',#1263,#1263,#1079,.F.);
#1506=EDGE_CURVE('',#1263,#1262,#876,.T.);
#1507=EDGE_CURVE('',#1257,#1263,#877,.T.);
#1508=EDGE_CURVE('',#1264,#1264,#1080,.T.);
#1509=EDGE_CURVE('',#1264,#1265,#878,.T.);
#1510=EDGE_CURVE('',#1265,#1265,#1081,.T.);
#1511=EDGE_CURVE('',#1266,#1266,#1082,.T.);
#1512=EDGE_CURVE('',#1267,#1267,#1083,.T.);
#1513=EDGE_CURVE('',#1267,#1268,#879,.T.);
#1514=EDGE_CURVE('',#1268,#1268,#1084,.T.);
#1515=EDGE_CURVE('',#1269,#1269,#1085,.T.);
#1516=EDGE_CURVE('',#1269,#1266,#880,.T.);
#1517=EDGE_CURVE('',#1270,#1270,#1086,.T.);
#1518=EDGE_CURVE('',#1270,#1271,#881,.T.);
#1519=EDGE_CURVE('',#1271,#1271,#1087,.T.);
#1520=EDGE_CURVE('',#1272,#1273,#1088,.T.);
#1521=EDGE_CURVE('',#1273,#1272,#1089,.T.);
#1522=EDGE_CURVE('',#1273,#1274,#1090,.T.);
#1523=EDGE_CURVE('',#1275,#1274,#1091,.T.);
#1524=EDGE_CURVE('',#1274,#1275,#1092,.T.);
#1525=EDGE_CURVE('',#1275,#1276,#882,.T.);
#1526=EDGE_CURVE('',#1276,#1276,#1093,.T.);
#1527=EDGE_CURVE('',#1277,#1277,#1094,.T.);
#1528=EDGE_CURVE('',#1277,#1278,#883,.T.);
#1529=EDGE_CURVE('',#1278,#1278,#1095,.T.);
#1530=EDGE_CURVE('',#1278,#1279,#884,.T.);
#1531=EDGE_CURVE('',#1279,#1279,#1096,.T.);
#1532=EDGE_CURVE('',#1280,#1280,#1097,.T.);
#1533=EDGE_CURVE('',#1280,#1272,#885,.T.);
#1534=EDGE_CURVE('',#1281,#1281,#1098,.T.);
#1535=EDGE_CURVE('',#1281,#1277,#886,.T.);
#1536=EDGE_CURVE('',#1282,#1283,#1099,.T.);
#1537=EDGE_CURVE('',#1283,#1282,#1100,.T.);
#1538=EDGE_CURVE('',#1283,#1284,#1101,.T.);
#1539=EDGE_CURVE('',#1285,#1284,#1102,.T.);
#1540=EDGE_CURVE('',#1284,#1285,#1103,.T.);
#1541=EDGE_CURVE('',#1286,#1286,#1104,.T.);
#1542=EDGE_CURVE('',#1286,#1285,#887,.T.);
#1543=EDGE_CURVE('',#1287,#1287,#1105,.T.);
#1544=EDGE_CURVE('',#1288,#1288,#1106,.T.);
#1545=EDGE_CURVE('',#1289,#1289,#1107,.T.);
#1546=EDGE_CURVE('',#1289,#1287,#888,.T.);
#1547=EDGE_CURVE('',#1290,#1290,#1108,.T.);
#1548=EDGE_CURVE('',#1290,#1289,#889,.T.);
#1549=EDGE_CURVE('',#1291,#1291,#1109,.T.);
#1550=EDGE_CURVE('',#1291,#1290,#890,.T.);
#1551=EDGE_CURVE('',#1282,#1288,#891,.T.);
#1552=EDGE_CURVE('',#1292,#1293,#1110,.T.);
#1553=EDGE_CURVE('',#1294,#1295,#1111,.T.);
#1554=EDGE_CURVE('',#1296,#1297,#1112,.T.);
#1555=EDGE_CURVE('',#1298,#1299,#1113,.T.);
#1556=EDGE_CURVE('',#1300,#1301,#1114,.T.);
#1557=EDGE_CURVE('',#1302,#1303,#1115,.T.);
#1558=EDGE_CURVE('',#1304,#1305,#1116,.T.);
#1559=EDGE_CURVE('',#1306,#1307,#11,.T.);
#1560=EDGE_CURVE('',#1308,#1306,#1117,.T.);
#1561=EDGE_CURVE('',#1309,#1308,#12,.T.);
#1562=EDGE_CURVE('',#1307,#1309,#1118,.T.);
#1563=EDGE_CURVE('',#1310,#1308,#1119,.T.);
#1564=EDGE_CURVE('',#1310,#1311,#13,.T.);
#1565=EDGE_CURVE('',#1312,#1311,#1120,.T.);
#1566=EDGE_CURVE('',#1312,#1313,#14,.T.);
#1567=EDGE_CURVE('',#1314,#1313,#1121,.T.);
#1568=EDGE_CURVE('',#1314,#1315,#892,.T.);
#1569=EDGE_CURVE('',#1315,#1315,#1122,.T.);
#1570=EDGE_CURVE('',#1316,#1314,#1123,.T.);
#1571=EDGE_CURVE('',#1316,#1317,#15,.T.);
#1572=EDGE_CURVE('',#1318,#1317,#1124,.T.);
#1573=EDGE_CURVE('',#1318,#1319,#16,.T.);
#1574=EDGE_CURVE('',#1320,#1319,#1125,.T.);
#1575=EDGE_CURVE('',#1320,#1321,#17,.T.);
#1576=EDGE_CURVE('',#1322,#1321,#1126,.T.);
#1577=EDGE_CURVE('',#1322,#1323,#18,.T.);
#1578=EDGE_CURVE('',#1309,#1323,#1127,.T.);
#1579=EDGE_CURVE('',#1306,#1324,#1128,.T.);
#1580=EDGE_CURVE('',#1324,#1310,#1129,.T.);
#1581=EDGE_CURVE('',#1325,#1324,#19,.T.);
#1582=EDGE_CURVE('',#1311,#1325,#1130,.T.);
#1583=EDGE_CURVE('',#1325,#1326,#1131,.T.);
#1584=EDGE_CURVE('',#1326,#1312,#1132,.T.);
#1585=EDGE_CURVE('',#1327,#1326,#20,.T.);
#1586=EDGE_CURVE('',#1313,#1327,#1133,.T.);
#1587=EDGE_CURVE('',#1327,#1328,#1134,.T.);
#1588=EDGE_CURVE('',#1328,#1329,#1135,.T.);
#1589=EDGE_CURVE('',#1329,#1316,#1136,.T.);
#1590=EDGE_CURVE('',#1330,#1329,#21,.T.);
#1591=EDGE_CURVE('',#1317,#1330,#1137,.T.);
#1592=EDGE_CURVE('',#1330,#1331,#1138,.T.);
#1593=EDGE_CURVE('',#1331,#1318,#1139,.T.);
#1594=EDGE_CURVE('',#1332,#1331,#22,.T.);
#1595=EDGE_CURVE('',#1319,#1332,#1140,.T.);
#1596=EDGE_CURVE('',#1332,#1333,#1141,.T.);
#1597=EDGE_CURVE('',#1333,#1320,#1142,.T.);
#1598=EDGE_CURVE('',#1334,#1333,#23,.T.);
#1599=EDGE_CURVE('',#1321,#1334,#1143,.T.);
#1600=EDGE_CURVE('',#1335,#1335,#1144,.T.);
#1601=EDGE_CURVE('',#1335,#1328,#893,.T.);
#1602=EDGE_CURVE('',#1336,#1307,#1145,.T.);
#1603=EDGE_CURVE('',#1336,#1337,#24,.T.);
#1604=EDGE_CURVE('',#1334,#1337,#1146,.T.);
#1605=EDGE_CURVE('',#1323,#1336,#1147,.T.);
#1606=EDGE_CURVE('',#1337,#1322,#1148,.T.);
#1607=EDGE_CURVE('',#1338,#1338,#1149,.T.);
#1608=EDGE_CURVE('',#1339,#1339,#1150,.T.);
#1609=EDGE_CURVE('',#1340,#1340,#1151,.T.);
#1610=EDGE_CURVE('',#1340,#1338,#894,.T.);
#1611=EDGE_CURVE('',#1341,#1341,#1152,.T.);
#1612=EDGE_CURVE('',#1341,#1339,#895,.T.);
#1613=EDGE_CURVE('',#1342,#1342,#1153,.T.);
#1614=EDGE_CURVE('',#1343,#1343,#1154,.T.);
#1615=EDGE_CURVE('',#1344,#1344,#1155,.T.);
#1616=EDGE_CURVE('',#1344,#1342,#896,.T.);
#1617=EDGE_CURVE('',#1345,#1345,#1156,.T.);
#1618=EDGE_CURVE('',#1345,#1343,#897,.T.);
#1619=EDGE_CURVE('',#1346,#1346,#1157,.T.);
#1620=EDGE_CURVE('',#1346,#1347,#898,.T.);
#1621=EDGE_CURVE('',#1347,#1347,#1158,.T.);
#1622=EDGE_CURVE('',#1348,#1348,#1159,.T.);
#1623=EDGE_CURVE('',#1348,#1349,#899,.T.);
#1624=EDGE_CURVE('',#1349,#1349,#1160,.T.);
#1625=ORIENTED_EDGE('',*,*,#1350,.F.);
#1626=ORIENTED_EDGE('',*,*,#1351,.T.);
#1627=ORIENTED_EDGE('',*,*,#1352,.F.);
#1628=ORIENTED_EDGE('',*,*,#1351,.F.);
#1629=ORIENTED_EDGE('',*,*,#1350,.T.);
#1630=ORIENTED_EDGE('',*,*,#1353,.F.);
#1631=ORIENTED_EDGE('',*,*,#1354,.T.);
#1632=ORIENTED_EDGE('',*,*,#1355,.F.);
#1633=ORIENTED_EDGE('',*,*,#1354,.F.);
#1634=ORIENTED_EDGE('',*,*,#1353,.T.);
#1635=ORIENTED_EDGE('',*,*,#1356,.F.);
#1636=ORIENTED_EDGE('',*,*,#1357,.T.);
#1637=ORIENTED_EDGE('',*,*,#1358,.T.);
#1638=ORIENTED_EDGE('',*,*,#1357,.F.);
#1639=ORIENTED_EDGE('',*,*,#1358,.F.);
#1640=ORIENTED_EDGE('',*,*,#1359,.F.);
#1641=ORIENTED_EDGE('',*,*,#1360,.T.);
#1642=ORIENTED_EDGE('',*,*,#1361,.T.);
#1643=ORIENTED_EDGE('',*,*,#1360,.F.);
#1644=ORIENTED_EDGE('',*,*,#1361,.F.);
#1645=ORIENTED_EDGE('',*,*,#1362,.T.);
#1646=ORIENTED_EDGE('',*,*,#1363,.T.);
#1647=ORIENTED_EDGE('',*,*,#1364,.F.);
#1648=ORIENTED_EDGE('',*,*,#1365,.F.);
#1649=ORIENTED_EDGE('',*,*,#1352,.T.);
#1650=ORIENTED_EDGE('',*,*,#1355,.T.);
#1651=ORIENTED_EDGE('',*,*,#1366,.T.);
#1652=ORIENTED_EDGE('',*,*,#1365,.T.);
#1653=ORIENTED_EDGE('',*,*,#1367,.F.);
#1654=ORIENTED_EDGE('',*,*,#1368,.F.);
#1655=ORIENTED_EDGE('',*,*,#1369,.T.);
#1656=ORIENTED_EDGE('',*,*,#1368,.T.);
#1657=ORIENTED_EDGE('',*,*,#1370,.F.);
#1658=ORIENTED_EDGE('',*,*,#1371,.F.);
#1659=ORIENTED_EDGE('',*,*,#1356,.T.);
#1660=ORIENTED_EDGE('',*,*,#1359,.T.);
#1661=ORIENTED_EDGE('',*,*,#1372,.T.);
#1662=ORIENTED_EDGE('',*,*,#1371,.T.);
#1663=ORIENTED_EDGE('',*,*,#1373,.F.);
#1664=ORIENTED_EDGE('',*,*,#1363,.F.);
#1665=ORIENTED_EDGE('',*,*,#1373,.T.);
#1666=ORIENTED_EDGE('',*,*,#1370,.T.);
#1667=ORIENTED_EDGE('',*,*,#1367,.T.);
#1668=ORIENTED_EDGE('',*,*,#1364,.T.);
#1669=ORIENTED_EDGE('',*,*,#1372,.F.);
#1670=ORIENTED_EDGE('',*,*,#1362,.F.);
#1671=ORIENTED_EDGE('',*,*,#1366,.F.);
#1672=ORIENTED_EDGE('',*,*,#1369,.F.);
#1673=ORIENTED_EDGE('',*,*,#1374,.F.);
#1674=ORIENTED_EDGE('',*,*,#1375,.T.);
#1675=ORIENTED_EDGE('',*,*,#1376,.F.);
#1676=ORIENTED_EDGE('',*,*,#1375,.F.);
#1677=ORIENTED_EDGE('',*,*,#1377,.F.);
#1678=ORIENTED_EDGE('',*,*,#1378,.T.);
#1679=ORIENTED_EDGE('',*,*,#1379,.F.);
#1680=ORIENTED_EDGE('',*,*,#1378,.F.);
#1681=ORIENTED_EDGE('',*,*,#1380,.F.);
#1682=ORIENTED_EDGE('',*,*,#1381,.T.);
#1683=ORIENTED_EDGE('',*,*,#1382,.F.);
#1684=ORIENTED_EDGE('',*,*,#1381,.F.);
#1685=ORIENTED_EDGE('',*,*,#1383,.F.);
#1686=ORIENTED_EDGE('',*,*,#1384,.T.);
#1687=ORIENTED_EDGE('',*,*,#1385,.F.);
#1688=ORIENTED_EDGE('',*,*,#1384,.F.);
#1689=ORIENTED_EDGE('',*,*,#1386,.T.);
#1690=ORIENTED_EDGE('',*,*,#1387,.T.);
#1691=ORIENTED_EDGE('',*,*,#1388,.F.);
#1692=ORIENTED_EDGE('',*,*,#1389,.F.);
#1693=ORIENTED_EDGE('',*,*,#1376,.T.);
#1694=ORIENTED_EDGE('',*,*,#1379,.T.);
#1695=ORIENTED_EDGE('',*,*,#1382,.T.);
#1696=ORIENTED_EDGE('',*,*,#1385,.T.);
#1697=ORIENTED_EDGE('',*,*,#1390,.T.);
#1698=ORIENTED_EDGE('',*,*,#1389,.T.);
#1699=ORIENTED_EDGE('',*,*,#1391,.F.);
#1700=ORIENTED_EDGE('',*,*,#1392,.F.);
#1701=ORIENTED_EDGE('',*,*,#1393,.T.);
#1702=ORIENTED_EDGE('',*,*,#1392,.T.);
#1703=ORIENTED_EDGE('',*,*,#1394,.F.);
#1704=ORIENTED_EDGE('',*,*,#1395,.F.);
#1705=ORIENTED_EDGE('',*,*,#1374,.T.);
#1706=ORIENTED_EDGE('',*,*,#1377,.T.);
#1707=ORIENTED_EDGE('',*,*,#1380,.T.);
#1708=ORIENTED_EDGE('',*,*,#1383,.T.);
#1709=ORIENTED_EDGE('',*,*,#1396,.T.);
#1710=ORIENTED_EDGE('',*,*,#1395,.T.);
#1711=ORIENTED_EDGE('',*,*,#1397,.F.);
#1712=ORIENTED_EDGE('',*,*,#1387,.F.);
#1713=ORIENTED_EDGE('',*,*,#1397,.T.);
#1714=ORIENTED_EDGE('',*,*,#1394,.T.);
#1715=ORIENTED_EDGE('',*,*,#1391,.T.);
#1716=ORIENTED_EDGE('',*,*,#1388,.T.);
#1717=ORIENTED_EDGE('',*,*,#1396,.F.);
#1718=ORIENTED_EDGE('',*,*,#1386,.F.);
#1719=ORIENTED_EDGE('',*,*,#1390,.F.);
#1720=ORIENTED_EDGE('',*,*,#1393,.F.);
#1721=ORIENTED_EDGE('',*,*,#1398,.F.);
#1722=ORIENTED_EDGE('',*,*,#1399,.T.);
#1723=ORIENTED_EDGE('',*,*,#1400,.F.);
#1724=ORIENTED_EDGE('',*,*,#1399,.F.);
#1725=ORIENTED_EDGE('',*,*,#1401,.F.);
#1726=ORIENTED_EDGE('',*,*,#1402,.T.);
#1727=ORIENTED_EDGE('',*,*,#1403,.F.);
#1728=ORIENTED_EDGE('',*,*,#1404,.F.);
#1729=ORIENTED_EDGE('',*,*,#1405,.F.);
#1730=ORIENTED_EDGE('',*,*,#1406,.F.);
#1731=ORIENTED_EDGE('',*,*,#1407,.F.);
#1732=ORIENTED_EDGE('',*,*,#1408,.F.);
#1733=ORIENTED_EDGE('',*,*,#1409,.F.);
#1734=ORIENTED_EDGE('',*,*,#1402,.F.);
#1735=ORIENTED_EDGE('',*,*,#1410,.F.);
#1736=ORIENTED_EDGE('',*,*,#1408,.T.);
#1737=ORIENTED_EDGE('',*,*,#1411,.T.);
#1738=ORIENTED_EDGE('',*,*,#1403,.T.);
#1739=ORIENTED_EDGE('',*,*,#1409,.T.);
#1740=ORIENTED_EDGE('',*,*,#1407,.T.);
#1741=ORIENTED_EDGE('',*,*,#1400,.T.);
#1742=ORIENTED_EDGE('',*,*,#1404,.T.);
#1743=ORIENTED_EDGE('',*,*,#1411,.F.);
#1744=ORIENTED_EDGE('',*,*,#1406,.T.);
#1745=ORIENTED_EDGE('',*,*,#1412,.T.);
#1746=ORIENTED_EDGE('',*,*,#1412,.F.);
#1747=ORIENTED_EDGE('',*,*,#1405,.T.);
#1748=ORIENTED_EDGE('',*,*,#1410,.T.);
#1749=ORIENTED_EDGE('',*,*,#1401,.T.);
#1750=ORIENTED_EDGE('',*,*,#1398,.T.);
#1751=ORIENTED_EDGE('',*,*,#1413,.F.);
#1752=ORIENTED_EDGE('',*,*,#1414,.T.);
#1753=ORIENTED_EDGE('',*,*,#1415,.T.);
#1754=ORIENTED_EDGE('',*,*,#1414,.F.);
#1755=ORIENTED_EDGE('',*,*,#1416,.F.);
#1756=ORIENTED_EDGE('',*,*,#1417,.T.);
#1757=ORIENTED_EDGE('',*,*,#1418,.T.);
#1758=ORIENTED_EDGE('',*,*,#1417,.F.);
#1759=ORIENTED_EDGE('',*,*,#1416,.T.);
#1760=ORIENTED_EDGE('',*,*,#1413,.T.);
#1761=ORIENTED_EDGE('',*,*,#1418,.F.);
#1762=ORIENTED_EDGE('',*,*,#1415,.F.);
#1763=ORIENTED_EDGE('',*,*,#1419,.F.);
#1764=ORIENTED_EDGE('',*,*,#1420,.F.);
#1765=ORIENTED_EDGE('',*,*,#1421,.T.);
#1766=ORIENTED_EDGE('',*,*,#1419,.T.);
#1767=ORIENTED_EDGE('',*,*,#1421,.F.);
#1768=ORIENTED_EDGE('',*,*,#1422,.F.);
#1769=ORIENTED_EDGE('',*,*,#1423,.T.);
#1770=ORIENTED_EDGE('',*,*,#1420,.T.);
#1771=ORIENTED_EDGE('',*,*,#1423,.F.);
#1772=ORIENTED_EDGE('',*,*,#1424,.F.);
#1773=ORIENTED_EDGE('',*,*,#1425,.T.);
#1774=ORIENTED_EDGE('',*,*,#1422,.T.);
#1775=ORIENTED_EDGE('',*,*,#1425,.F.);
#1776=ORIENTED_EDGE('',*,*,#1424,.T.);
#1777=ORIENTED_EDGE('',*,*,#1426,.F.);
#1778=ORIENTED_EDGE('',*,*,#1427,.F.);
#1779=ORIENTED_EDGE('',*,*,#1428,.T.);
#1780=ORIENTED_EDGE('',*,*,#1426,.T.);
#1781=ORIENTED_EDGE('',*,*,#1428,.F.);
#1782=ORIENTED_EDGE('',*,*,#1429,.F.);
#1783=ORIENTED_EDGE('',*,*,#1430,.T.);
#1784=ORIENTED_EDGE('',*,*,#1427,.T.);
#1785=ORIENTED_EDGE('',*,*,#1430,.F.);
#1786=ORIENTED_EDGE('',*,*,#1431,.F.);
#1787=ORIENTED_EDGE('',*,*,#1432,.T.);
#1788=ORIENTED_EDGE('',*,*,#1429,.T.);
#1789=ORIENTED_EDGE('',*,*,#1432,.F.);
#1790=ORIENTED_EDGE('',*,*,#1431,.T.);
#1791=ORIENTED_EDGE('',*,*,#1433,.T.);
#1792=ORIENTED_EDGE('',*,*,#1434,.T.);
#1793=ORIENTED_EDGE('',*,*,#1435,.T.);
#1794=ORIENTED_EDGE('',*,*,#1436,.F.);
#1795=ORIENTED_EDGE('',*,*,#1437,.T.);
#1796=ORIENTED_EDGE('',*,*,#1438,.T.);
#1797=ORIENTED_EDGE('',*,*,#1439,.T.);
#1798=ORIENTED_EDGE('',*,*,#1434,.F.);
#1799=ORIENTED_EDGE('',*,*,#1440,.T.);
#1800=ORIENTED_EDGE('',*,*,#1441,.T.);
#1801=ORIENTED_EDGE('',*,*,#1442,.T.);
#1802=ORIENTED_EDGE('',*,*,#1438,.F.);
#1803=ORIENTED_EDGE('',*,*,#1443,.T.);
#1804=ORIENTED_EDGE('',*,*,#1444,.T.);
#1805=ORIENTED_EDGE('',*,*,#1445,.T.);
#1806=ORIENTED_EDGE('',*,*,#1441,.F.);
#1807=ORIENTED_EDGE('',*,*,#1446,.T.);
#1808=ORIENTED_EDGE('',*,*,#1447,.T.);
#1809=ORIENTED_EDGE('',*,*,#1448,.T.);
#1810=ORIENTED_EDGE('',*,*,#1444,.F.);
#1811=ORIENTED_EDGE('',*,*,#1449,.T.);
#1812=ORIENTED_EDGE('',*,*,#1436,.T.);
#1813=ORIENTED_EDGE('',*,*,#1450,.T.);
#1814=ORIENTED_EDGE('',*,*,#1447,.F.);
#1815=ORIENTED_EDGE('',*,*,#1449,.F.);
#1816=ORIENTED_EDGE('',*,*,#1446,.F.);
#1817=ORIENTED_EDGE('',*,*,#1443,.F.);
#1818=ORIENTED_EDGE('',*,*,#1440,.F.);
#1819=ORIENTED_EDGE('',*,*,#1437,.F.);
#1820=ORIENTED_EDGE('',*,*,#1433,.F.);
#1821=ORIENTED_EDGE('',*,*,#1450,.F.);
#1822=ORIENTED_EDGE('',*,*,#1435,.F.);
#1823=ORIENTED_EDGE('',*,*,#1439,.F.);
#1824=ORIENTED_EDGE('',*,*,#1442,.F.);
#1825=ORIENTED_EDGE('',*,*,#1445,.F.);
#1826=ORIENTED_EDGE('',*,*,#1448,.F.);
#1827=ORIENTED_EDGE('',*,*,#1451,.F.);
#1828=ORIENTED_EDGE('',*,*,#1452,.T.);
#1829=ORIENTED_EDGE('',*,*,#1453,.T.);
#1830=ORIENTED_EDGE('',*,*,#1452,.F.);
#1831=ORIENTED_EDGE('',*,*,#1453,.F.);
#1832=ORIENTED_EDGE('',*,*,#1454,.F.);
#1833=ORIENTED_EDGE('',*,*,#1455,.T.);
#1834=ORIENTED_EDGE('',*,*,#1456,.F.);
#1835=ORIENTED_EDGE('',*,*,#1457,.T.);
#1836=ORIENTED_EDGE('',*,*,#1454,.T.);
#1837=ORIENTED_EDGE('',*,*,#1457,.F.);
#1838=ORIENTED_EDGE('',*,*,#1456,.T.);
#1839=ORIENTED_EDGE('',*,*,#1455,.F.);
#1840=ORIENTED_EDGE('',*,*,#1458,.T.);
#1841=ORIENTED_EDGE('',*,*,#1459,.T.);
#1842=ORIENTED_EDGE('',*,*,#1458,.F.);
#1843=ORIENTED_EDGE('',*,*,#1459,.F.);
#1844=ORIENTED_EDGE('',*,*,#1451,.T.);
#1845=ORIENTED_EDGE('',*,*,#1460,.F.);
#1846=ORIENTED_EDGE('',*,*,#1461,.T.);
#1847=ORIENTED_EDGE('',*,*,#1462,.T.);
#1848=ORIENTED_EDGE('',*,*,#1461,.F.);
#1849=ORIENTED_EDGE('',*,*,#1463,.F.);
#1850=ORIENTED_EDGE('',*,*,#1464,.T.);
#1851=ORIENTED_EDGE('',*,*,#1465,.T.);
#1852=ORIENTED_EDGE('',*,*,#1464,.F.);
#1853=ORIENTED_EDGE('',*,*,#1463,.T.);
#1854=ORIENTED_EDGE('',*,*,#1460,.T.);
#1855=ORIENTED_EDGE('',*,*,#1465,.F.);
#1856=ORIENTED_EDGE('',*,*,#1462,.F.);
#1857=ORIENTED_EDGE('',*,*,#1466,.F.);
#1858=ORIENTED_EDGE('',*,*,#1467,.T.);
#1859=ORIENTED_EDGE('',*,*,#1468,.T.);
#1860=ORIENTED_EDGE('',*,*,#1467,.F.);
#1861=ORIENTED_EDGE('',*,*,#1469,.F.);
#1862=ORIENTED_EDGE('',*,*,#1470,.T.);
#1863=ORIENTED_EDGE('',*,*,#1471,.T.);
#1864=ORIENTED_EDGE('',*,*,#1470,.F.);
#1865=ORIENTED_EDGE('',*,*,#1469,.T.);
#1866=ORIENTED_EDGE('',*,*,#1466,.T.);
#1867=ORIENTED_EDGE('',*,*,#1471,.F.);
#1868=ORIENTED_EDGE('',*,*,#1468,.F.);
#1869=ORIENTED_EDGE('',*,*,#1472,.F.);
#1870=ORIENTED_EDGE('',*,*,#1473,.T.);
#1871=ORIENTED_EDGE('',*,*,#1474,.T.);
#1872=ORIENTED_EDGE('',*,*,#1473,.F.);
#1873=ORIENTED_EDGE('',*,*,#1475,.F.);
#1874=ORIENTED_EDGE('',*,*,#1476,.T.);
#1875=ORIENTED_EDGE('',*,*,#1477,.T.);
#1876=ORIENTED_EDGE('',*,*,#1476,.F.);
#1877=ORIENTED_EDGE('',*,*,#1475,.T.);
#1878=ORIENTED_EDGE('',*,*,#1472,.T.);
#1879=ORIENTED_EDGE('',*,*,#1477,.F.);
#1880=ORIENTED_EDGE('',*,*,#1474,.F.);
#1881=ORIENTED_EDGE('',*,*,#1478,.T.);
#1882=ORIENTED_EDGE('',*,*,#1479,.T.);
#1883=ORIENTED_EDGE('',*,*,#1480,.T.);
#1884=ORIENTED_EDGE('',*,*,#1481,.F.);
#1885=ORIENTED_EDGE('',*,*,#1482,.T.);
#1886=ORIENTED_EDGE('',*,*,#1483,.T.);
#1887=ORIENTED_EDGE('',*,*,#1484,.T.);
#1888=ORIENTED_EDGE('',*,*,#1479,.F.);
#1889=ORIENTED_EDGE('',*,*,#1485,.T.);
#1890=ORIENTED_EDGE('',*,*,#1486,.T.);
#1891=ORIENTED_EDGE('',*,*,#1487,.T.);
#1892=ORIENTED_EDGE('',*,*,#1483,.F.);
#1893=ORIENTED_EDGE('',*,*,#1488,.T.);
#1894=ORIENTED_EDGE('',*,*,#1489,.T.);
#1895=ORIENTED_EDGE('',*,*,#1490,.T.);
#1896=ORIENTED_EDGE('',*,*,#1486,.F.);
#1897=ORIENTED_EDGE('',*,*,#1491,.T.);
#1898=ORIENTED_EDGE('',*,*,#1492,.T.);
#1899=ORIENTED_EDGE('',*,*,#1493,.T.);
#1900=ORIENTED_EDGE('',*,*,#1489,.F.);
#1901=ORIENTED_EDGE('',*,*,#1494,.T.);
#1902=ORIENTED_EDGE('',*,*,#1481,.T.);
#1903=ORIENTED_EDGE('',*,*,#1495,.T.);
#1904=ORIENTED_EDGE('',*,*,#1492,.F.);
#1905=ORIENTED_EDGE('',*,*,#1494,.F.);
#1906=ORIENTED_EDGE('',*,*,#1491,.F.);
#1907=ORIENTED_EDGE('',*,*,#1488,.F.);
#1908=ORIENTED_EDGE('',*,*,#1485,.F.);
#1909=ORIENTED_EDGE('',*,*,#1482,.F.);
#1910=ORIENTED_EDGE('',*,*,#1478,.F.);
#1911=ORIENTED_EDGE('',*,*,#1495,.F.);
#1912=ORIENTED_EDGE('',*,*,#1480,.F.);
#1913=ORIENTED_EDGE('',*,*,#1484,.F.);
#1914=ORIENTED_EDGE('',*,*,#1487,.F.);
#1915=ORIENTED_EDGE('',*,*,#1490,.F.);
#1916=ORIENTED_EDGE('',*,*,#1493,.F.);
#1917=ORIENTED_EDGE('',*,*,#1496,.F.);
#1918=ORIENTED_EDGE('',*,*,#1497,.F.);
#1919=ORIENTED_EDGE('',*,*,#1498,.F.);
#1920=ORIENTED_EDGE('',*,*,#1499,.T.);
#1921=ORIENTED_EDGE('',*,*,#1497,.T.);
#1922=ORIENTED_EDGE('',*,*,#1499,.F.);
#1923=ORIENTED_EDGE('',*,*,#1500,.F.);
#1924=ORIENTED_EDGE('',*,*,#1501,.T.);
#1925=ORIENTED_EDGE('',*,*,#1498,.T.);
#1926=ORIENTED_EDGE('',*,*,#1501,.F.);
#1927=ORIENTED_EDGE('',*,*,#1502,.F.);
#1928=ORIENTED_EDGE('',*,*,#1503,.T.);
#1929=ORIENTED_EDGE('',*,*,#1500,.T.);
#1930=ORIENTED_EDGE('',*,*,#1503,.F.);
#1931=ORIENTED_EDGE('',*,*,#1502,.T.);
#1932=ORIENTED_EDGE('',*,*,#1504,.F.);
#1933=ORIENTED_EDGE('',*,*,#1505,.F.);
#1934=ORIENTED_EDGE('',*,*,#1506,.T.);
#1935=ORIENTED_EDGE('',*,*,#1504,.T.);
#1936=ORIENTED_EDGE('',*,*,#1506,.F.);
#1937=ORIENTED_EDGE('',*,*,#1496,.T.);
#1938=ORIENTED_EDGE('',*,*,#1507,.T.);
#1939=ORIENTED_EDGE('',*,*,#1505,.T.);
#1940=ORIENTED_EDGE('',*,*,#1507,.F.);
#1941=ORIENTED_EDGE('',*,*,#1508,.F.);
#1942=ORIENTED_EDGE('',*,*,#1509,.T.);
#1943=ORIENTED_EDGE('',*,*,#1510,.F.);
#1944=ORIENTED_EDGE('',*,*,#1509,.F.);
#1945=ORIENTED_EDGE('',*,*,#1508,.T.);
#1946=ORIENTED_EDGE('',*,*,#1511,.F.);
#1947=ORIENTED_EDGE('',*,*,#1512,.F.);
#1948=ORIENTED_EDGE('',*,*,#1513,.T.);
#1949=ORIENTED_EDGE('',*,*,#1514,.T.);
#1950=ORIENTED_EDGE('',*,*,#1513,.F.);
#1951=ORIENTED_EDGE('',*,*,#1514,.F.);
#1952=ORIENTED_EDGE('',*,*,#1515,.F.);
#1953=ORIENTED_EDGE('',*,*,#1515,.T.);
#1954=ORIENTED_EDGE('',*,*,#1516,.T.);
#1955=ORIENTED_EDGE('',*,*,#1511,.T.);
#1956=ORIENTED_EDGE('',*,*,#1516,.F.);
#1957=ORIENTED_EDGE('',*,*,#1517,.F.);
#1958=ORIENTED_EDGE('',*,*,#1518,.T.);
#1959=ORIENTED_EDGE('',*,*,#1519,.T.);
#1960=ORIENTED_EDGE('',*,*,#1518,.F.);
#1961=ORIENTED_EDGE('',*,*,#1517,.T.);
#1962=ORIENTED_EDGE('',*,*,#1510,.T.);
#1963=ORIENTED_EDGE('',*,*,#1519,.F.);
#1964=ORIENTED_EDGE('',*,*,#1512,.T.);
#1965=ORIENTED_EDGE('',*,*,#1520,.F.);
#1966=ORIENTED_EDGE('',*,*,#1521,.F.);
#1967=ORIENTED_EDGE('',*,*,#1522,.T.);
#1968=ORIENTED_EDGE('',*,*,#1523,.F.);
#1969=ORIENTED_EDGE('',*,*,#1524,.F.);
#1970=ORIENTED_EDGE('',*,*,#1522,.F.);
#1971=ORIENTED_EDGE('',*,*,#1523,.T.);
#1972=ORIENTED_EDGE('',*,*,#1524,.T.);
#1973=ORIENTED_EDGE('',*,*,#1525,.T.);
#1974=ORIENTED_EDGE('',*,*,#1526,.T.);
#1975=ORIENTED_EDGE('',*,*,#1525,.F.);
#1976=ORIENTED_EDGE('',*,*,#1527,.T.);
#1977=ORIENTED_EDGE('',*,*,#1528,.T.);
#1978=ORIENTED_EDGE('',*,*,#1529,.F.);
#1979=ORIENTED_EDGE('',*,*,#1528,.F.);
#1980=ORIENTED_EDGE('',*,*,#1529,.T.);
#1981=ORIENTED_EDGE('',*,*,#1530,.T.);
#1982=ORIENTED_EDGE('',*,*,#1531,.F.);
#1983=ORIENTED_EDGE('',*,*,#1530,.F.);
#1984=ORIENTED_EDGE('',*,*,#1526,.F.);
#1985=ORIENTED_EDGE('',*,*,#1531,.T.);
#1986=ORIENTED_EDGE('',*,*,#1532,.F.);
#1987=ORIENTED_EDGE('',*,*,#1533,.T.);
#1988=ORIENTED_EDGE('',*,*,#1520,.T.);
#1989=ORIENTED_EDGE('',*,*,#1521,.T.);
#1990=ORIENTED_EDGE('',*,*,#1533,.F.);
#1991=ORIENTED_EDGE('',*,*,#1532,.T.);
#1992=ORIENTED_EDGE('',*,*,#1534,.F.);
#1993=ORIENTED_EDGE('',*,*,#1534,.T.);
#1994=ORIENTED_EDGE('',*,*,#1535,.T.);
#1995=ORIENTED_EDGE('',*,*,#1527,.F.);
#1996=ORIENTED_EDGE('',*,*,#1535,.F.);
#1997=ORIENTED_EDGE('',*,*,#1536,.F.);
#1998=ORIENTED_EDGE('',*,*,#1537,.F.);
#1999=ORIENTED_EDGE('',*,*,#1538,.T.);
#2000=ORIENTED_EDGE('',*,*,#1539,.F.);
#2001=ORIENTED_EDGE('',*,*,#1540,.F.);
#2002=ORIENTED_EDGE('',*,*,#1538,.F.);
#2003=ORIENTED_EDGE('',*,*,#1541,.T.);
#2004=ORIENTED_EDGE('',*,*,#1542,.T.);
#2005=ORIENTED_EDGE('',*,*,#1539,.T.);
#2006=ORIENTED_EDGE('',*,*,#1540,.T.);
#2007=ORIENTED_EDGE('',*,*,#1542,.F.);
#2008=ORIENTED_EDGE('',*,*,#1543,.F.);
#2009=ORIENTED_EDGE('',*,*,#1544,.T.);
#2010=ORIENTED_EDGE('',*,*,#1545,.F.);
#2011=ORIENTED_EDGE('',*,*,#1546,.T.);
#2012=ORIENTED_EDGE('',*,*,#1543,.T.);
#2013=ORIENTED_EDGE('',*,*,#1546,.F.);
#2014=ORIENTED_EDGE('',*,*,#1547,.F.);
#2015=ORIENTED_EDGE('',*,*,#1548,.T.);
#2016=ORIENTED_EDGE('',*,*,#1545,.T.);
#2017=ORIENTED_EDGE('',*,*,#1548,.F.);
#2018=ORIENTED_EDGE('',*,*,#1549,.F.);
#2019=ORIENTED_EDGE('',*,*,#1550,.T.);
#2020=ORIENTED_EDGE('',*,*,#1547,.T.);
#2021=ORIENTED_EDGE('',*,*,#1550,.F.);
#2022=ORIENTED_EDGE('',*,*,#1549,.T.);
#2023=ORIENTED_EDGE('',*,*,#1541,.F.);
#2024=ORIENTED_EDGE('',*,*,#1536,.T.);
#2025=ORIENTED_EDGE('',*,*,#1537,.T.);
#2026=ORIENTED_EDGE('',*,*,#1551,.T.);
#2027=ORIENTED_EDGE('',*,*,#1544,.F.);
#2028=ORIENTED_EDGE('',*,*,#1551,.F.);
#2029=ORIENTED_EDGE('',*,*,#1552,.T.);
#2030=ORIENTED_EDGE('',*,*,#1552,.F.);
#2031=ORIENTED_EDGE('',*,*,#1553,.T.);
#2032=ORIENTED_EDGE('',*,*,#1553,.F.);
#2033=ORIENTED_EDGE('',*,*,#1554,.T.);
#2034=ORIENTED_EDGE('',*,*,#1554,.F.);
#2035=ORIENTED_EDGE('',*,*,#1555,.T.);
#2036=ORIENTED_EDGE('',*,*,#1555,.F.);
#2037=ORIENTED_EDGE('',*,*,#1556,.T.);
#2038=ORIENTED_EDGE('',*,*,#1556,.F.);
#2039=ORIENTED_EDGE('',*,*,#1557,.T.);
#2040=ORIENTED_EDGE('',*,*,#1557,.F.);
#2041=ORIENTED_EDGE('',*,*,#1558,.T.);
#2042=ORIENTED_EDGE('',*,*,#1558,.F.);
#2043=ORIENTED_EDGE('',*,*,#1559,.F.);
#2044=ORIENTED_EDGE('',*,*,#1560,.F.);
#2045=ORIENTED_EDGE('',*,*,#1561,.F.);
#2046=ORIENTED_EDGE('',*,*,#1562,.F.);
#2047=ORIENTED_EDGE('',*,*,#1561,.T.);
#2048=ORIENTED_EDGE('',*,*,#1563,.F.);
#2049=ORIENTED_EDGE('',*,*,#1564,.T.);
#2050=ORIENTED_EDGE('',*,*,#1565,.F.);
#2051=ORIENTED_EDGE('',*,*,#1566,.T.);
#2052=ORIENTED_EDGE('',*,*,#1567,.F.);
#2053=ORIENTED_EDGE('',*,*,#1568,.T.);
#2054=ORIENTED_EDGE('',*,*,#1569,.F.);
#2055=ORIENTED_EDGE('',*,*,#1568,.F.);
#2056=ORIENTED_EDGE('',*,*,#1570,.F.);
#2057=ORIENTED_EDGE('',*,*,#1571,.T.);
#2058=ORIENTED_EDGE('',*,*,#1572,.F.);
#2059=ORIENTED_EDGE('',*,*,#1573,.T.);
#2060=ORIENTED_EDGE('',*,*,#1574,.F.);
#2061=ORIENTED_EDGE('',*,*,#1575,.T.);
#2062=ORIENTED_EDGE('',*,*,#1576,.F.);
#2063=ORIENTED_EDGE('',*,*,#1577,.T.);
#2064=ORIENTED_EDGE('',*,*,#1578,.F.);
#2065=ORIENTED_EDGE('',*,*,#1560,.T.);
#2066=ORIENTED_EDGE('',*,*,#1579,.T.);
#2067=ORIENTED_EDGE('',*,*,#1580,.T.);
#2068=ORIENTED_EDGE('',*,*,#1563,.T.);
#2069=ORIENTED_EDGE('',*,*,#1581,.F.);
#2070=ORIENTED_EDGE('',*,*,#1582,.F.);
#2071=ORIENTED_EDGE('',*,*,#1564,.F.);
#2072=ORIENTED_EDGE('',*,*,#1580,.F.);
#2073=ORIENTED_EDGE('',*,*,#1582,.T.);
#2074=ORIENTED_EDGE('',*,*,#1583,.T.);
#2075=ORIENTED_EDGE('',*,*,#1584,.T.);
#2076=ORIENTED_EDGE('',*,*,#1565,.T.);
#2077=ORIENTED_EDGE('',*,*,#1585,.F.);
#2078=ORIENTED_EDGE('',*,*,#1586,.F.);
#2079=ORIENTED_EDGE('',*,*,#1566,.F.);
#2080=ORIENTED_EDGE('',*,*,#1584,.F.);
#2081=ORIENTED_EDGE('',*,*,#1586,.T.);
#2082=ORIENTED_EDGE('',*,*,#1587,.T.);
#2083=ORIENTED_EDGE('',*,*,#1588,.T.);
#2084=ORIENTED_EDGE('',*,*,#1589,.T.);
#2085=ORIENTED_EDGE('',*,*,#1570,.T.);
#2086=ORIENTED_EDGE('',*,*,#1567,.T.);
#2087=ORIENTED_EDGE('',*,*,#1590,.F.);
#2088=ORIENTED_EDGE('',*,*,#1591,.F.);
#2089=ORIENTED_EDGE('',*,*,#1571,.F.);
#2090=ORIENTED_EDGE('',*,*,#1589,.F.);
#2091=ORIENTED_EDGE('',*,*,#1591,.T.);
#2092=ORIENTED_EDGE('',*,*,#1592,.T.);
#2093=ORIENTED_EDGE('',*,*,#1593,.T.);
#2094=ORIENTED_EDGE('',*,*,#1572,.T.);
#2095=ORIENTED_EDGE('',*,*,#1594,.F.);
#2096=ORIENTED_EDGE('',*,*,#1595,.F.);
#2097=ORIENTED_EDGE('',*,*,#1573,.F.);
#2098=ORIENTED_EDGE('',*,*,#1593,.F.);
#2099=ORIENTED_EDGE('',*,*,#1595,.T.);
#2100=ORIENTED_EDGE('',*,*,#1596,.T.);
#2101=ORIENTED_EDGE('',*,*,#1597,.T.);
#2102=ORIENTED_EDGE('',*,*,#1574,.T.);
#2103=ORIENTED_EDGE('',*,*,#1575,.F.);
#2104=ORIENTED_EDGE('',*,*,#1597,.F.);
#2105=ORIENTED_EDGE('',*,*,#1598,.F.);
#2106=ORIENTED_EDGE('',*,*,#1599,.F.);
#2107=ORIENTED_EDGE('',*,*,#1600,.F.);
#2108=ORIENTED_EDGE('',*,*,#1601,.T.);
#2109=ORIENTED_EDGE('',*,*,#1587,.F.);
#2110=ORIENTED_EDGE('',*,*,#1585,.T.);
#2111=ORIENTED_EDGE('',*,*,#1583,.F.);
#2112=ORIENTED_EDGE('',*,*,#1581,.T.);
#2113=ORIENTED_EDGE('',*,*,#1579,.F.);
#2114=ORIENTED_EDGE('',*,*,#1559,.T.);
#2115=ORIENTED_EDGE('',*,*,#1602,.F.);
#2116=ORIENTED_EDGE('',*,*,#1603,.T.);
#2117=ORIENTED_EDGE('',*,*,#1604,.F.);
#2118=ORIENTED_EDGE('',*,*,#1598,.T.);
#2119=ORIENTED_EDGE('',*,*,#1596,.F.);
#2120=ORIENTED_EDGE('',*,*,#1594,.T.);
#2121=ORIENTED_EDGE('',*,*,#1592,.F.);
#2122=ORIENTED_EDGE('',*,*,#1590,.T.);
#2123=ORIENTED_EDGE('',*,*,#1588,.F.);
#2124=ORIENTED_EDGE('',*,*,#1601,.F.);
#2125=ORIENTED_EDGE('',*,*,#1562,.T.);
#2126=ORIENTED_EDGE('',*,*,#1578,.T.);
#2127=ORIENTED_EDGE('',*,*,#1605,.T.);
#2128=ORIENTED_EDGE('',*,*,#1602,.T.);
#2129=ORIENTED_EDGE('',*,*,#1577,.F.);
#2130=ORIENTED_EDGE('',*,*,#1606,.F.);
#2131=ORIENTED_EDGE('',*,*,#1603,.F.);
#2132=ORIENTED_EDGE('',*,*,#1605,.F.);
#2133=ORIENTED_EDGE('',*,*,#1569,.T.);
#2134=ORIENTED_EDGE('',*,*,#1600,.T.);
#2135=ORIENTED_EDGE('',*,*,#1599,.T.);
#2136=ORIENTED_EDGE('',*,*,#1604,.T.);
#2137=ORIENTED_EDGE('',*,*,#1606,.T.);
#2138=ORIENTED_EDGE('',*,*,#1576,.T.);
#2139=ORIENTED_EDGE('',*,*,#1607,.F.);
#2140=ORIENTED_EDGE('',*,*,#1608,.T.);
#2141=ORIENTED_EDGE('',*,*,#1609,.F.);
#2142=ORIENTED_EDGE('',*,*,#1610,.T.);
#2143=ORIENTED_EDGE('',*,*,#1607,.T.);
#2144=ORIENTED_EDGE('',*,*,#1610,.F.);
#2145=ORIENTED_EDGE('',*,*,#1609,.T.);
#2146=ORIENTED_EDGE('',*,*,#1611,.F.);
#2147=ORIENTED_EDGE('',*,*,#1611,.T.);
#2148=ORIENTED_EDGE('',*,*,#1612,.T.);
#2149=ORIENTED_EDGE('',*,*,#1608,.F.);
#2150=ORIENTED_EDGE('',*,*,#1612,.F.);
#2151=ORIENTED_EDGE('',*,*,#1613,.F.);
#2152=ORIENTED_EDGE('',*,*,#1614,.T.);
#2153=ORIENTED_EDGE('',*,*,#1615,.F.);
#2154=ORIENTED_EDGE('',*,*,#1616,.T.);
#2155=ORIENTED_EDGE('',*,*,#1613,.T.);
#2156=ORIENTED_EDGE('',*,*,#1616,.F.);
#2157=ORIENTED_EDGE('',*,*,#1615,.T.);
#2158=ORIENTED_EDGE('',*,*,#1617,.F.);
#2159=ORIENTED_EDGE('',*,*,#1617,.T.);
#2160=ORIENTED_EDGE('',*,*,#1618,.T.);
#2161=ORIENTED_EDGE('',*,*,#1614,.F.);
#2162=ORIENTED_EDGE('',*,*,#1618,.F.);
#2163=ORIENTED_EDGE('',*,*,#1619,.F.);
#2164=ORIENTED_EDGE('',*,*,#1620,.T.);
#2165=ORIENTED_EDGE('',*,*,#1621,.T.);
#2166=ORIENTED_EDGE('',*,*,#1620,.F.);
#2167=ORIENTED_EDGE('',*,*,#1622,.F.);
#2168=ORIENTED_EDGE('',*,*,#1623,.T.);
#2169=ORIENTED_EDGE('',*,*,#1624,.T.);
#2170=ORIENTED_EDGE('',*,*,#1623,.F.);
#2171=ORIENTED_EDGE('',*,*,#1622,.T.);
#2172=ORIENTED_EDGE('',*,*,#1619,.T.);
#2173=ORIENTED_EDGE('',*,*,#1624,.F.);
#2174=ORIENTED_EDGE('',*,*,#1621,.F.);
#2175=CYLINDRICAL_SURFACE('',#2582,0.34);
#2176=CYLINDRICAL_SURFACE('',#2586,0.34);
#2177=CYLINDRICAL_SURFACE('',#2590,0.34);
#2178=CYLINDRICAL_SURFACE('',#2594,0.34);
#2179=CYLINDRICAL_SURFACE('',#2605,0.425);
#2180=CYLINDRICAL_SURFACE('',#2608,0.425);
#2181=CYLINDRICAL_SURFACE('',#2611,0.6);
#2182=CYLINDRICAL_SURFACE('',#2614,0.6);
#2183=CYLINDRICAL_SURFACE('',#2624,0.510000000000002);
#2184=CYLINDRICAL_SURFACE('',#2632,2.);
#2185=CYLINDRICAL_SURFACE('',#2636,0.42);
#2186=CYLINDRICAL_SURFACE('',#2639,0.8);
#2187=CYLINDRICAL_SURFACE('',#2649,0.65);
#2188=CYLINDRICAL_SURFACE('',#2657,0.3933);
#2189=CYLINDRICAL_SURFACE('',#2671,0.165);
#2190=CYLINDRICAL_SURFACE('',#2678,1.);
#2191=CYLINDRICAL_SURFACE('',#2681,0.6);
#2192=CYLINDRICAL_SURFACE('',#2685,0.605);
#2193=CYLINDRICAL_SURFACE('',#2688,0.8);
#2194=CYLINDRICAL_SURFACE('',#2694,0.605);
#2195=CYLINDRICAL_SURFACE('',#2697,0.8);
#2196=CYLINDRICAL_SURFACE('',#2703,0.225);
#2197=CYLINDRICAL_SURFACE('',#2706,0.8);
#2198=CYLINDRICAL_SURFACE('',#2726,0.35);
#2199=CYLINDRICAL_SURFACE('',#2734,0.1954);
#2200=CYLINDRICAL_SURFACE('',#2769,1.6);
#2201=CYLINDRICAL_SURFACE('',#2774,1.6);
#2202=CYLINDRICAL_SURFACE('',#2779,0.62);
#2203=CYLINDRICAL_SURFACE('',#2780,3.75);
#2204=CYLINDRICAL_SURFACE('',#2793,1.070235);
#2205=CYLINDRICAL_SURFACE('',#2795,0.6);
#2206=CYLINDRICAL_SURFACE('',#2801,1.070235);
#2207=CYLINDRICAL_SURFACE('',#2813,1.129765);
#2208=CYLINDRICAL_SURFACE('',#2820,1.6);
#2209=CYLINDRICAL_SURFACE('',#2825,1.129765);
#2210=CYLINDRICAL_SURFACE('',#2845,1.123812);
#2211=CYLINDRICAL_SURFACE('',#2881,1.076188);
#2212=CYLINDRICAL_SURFACE('',#2895,1.119765);
#2213=CYLINDRICAL_SURFACE('',#2899,1.085235);
#2214=CYLINDRICAL_SURFACE('',#2903,1.119765);
#2215=CYLINDRICAL_SURFACE('',#2907,1.085235);
#2216=CYLINDRICAL_SURFACE('',#2914,1.2);
#2217=CYLINDRICAL_SURFACE('',#2917,1.6);
#2218=ADVANCED_FACE('',(#442),#2175,.F.);
#2219=ADVANCED_FACE('',(#443),#365,.T.);
#2220=ADVANCED_FACE('',(#444),#2176,.F.);
#2221=ADVANCED_FACE('',(#445),#366,.T.);
#2222=ADVANCED_FACE('',(#446),#2177,.F.);
#2223=ADVANCED_FACE('',(#447),#367,.F.);
#2224=ADVANCED_FACE('',(#448),#2178,.F.);
#2225=ADVANCED_FACE('',(#449),#368,.F.);
#2226=ADVANCED_FACE('',(#450,#324,#325),#369,.T.);
#2227=ADVANCED_FACE('',(#451),#370,.T.);
#2228=ADVANCED_FACE('',(#452,#326,#327),#371,.T.);
#2229=ADVANCED_FACE('',(#453),#372,.T.);
#2230=ADVANCED_FACE('',(#454),#373,.T.);
#2231=ADVANCED_FACE('',(#455),#374,.F.);
#2232=ADVANCED_FACE('',(#456),#2179,.F.);
#2233=ADVANCED_FACE('',(#457),#2180,.F.);
#2234=ADVANCED_FACE('',(#458),#2181,.F.);
#2235=ADVANCED_FACE('',(#459),#2182,.F.);
#2236=ADVANCED_FACE('',(#460,#328,#329,#330,#331),#375,.T.);
#2237=ADVANCED_FACE('',(#461),#376,.T.);
#2238=ADVANCED_FACE('',(#462,#332,#333,#334,#335),#377,.T.);
#2239=ADVANCED_FACE('',(#463),#378,.T.);
#2240=ADVANCED_FACE('',(#464),#379,.T.);
#2241=ADVANCED_FACE('',(#465),#380,.F.);
#2242=ADVANCED_FACE('',(#466),#2183,.F.);
#2243=ADVANCED_FACE('',(#467),#381,.T.);
#2244=ADVANCED_FACE('',(#468),#382,.T.);
#2245=ADVANCED_FACE('',(#469),#383,.T.);
#2246=ADVANCED_FACE('',(#470,#336),#384,.T.);
#2247=ADVANCED_FACE('',(#471),#2184,.T.);
#2248=ADVANCED_FACE('',(#472,#337),#385,.F.);
#2249=ADVANCED_FACE('',(#473),#2185,.F.);
#2250=ADVANCED_FACE('',(#474),#2186,.T.);
#2251=ADVANCED_FACE('',(#475,#338),#386,.T.);
#2252=ADVANCED_FACE('',(#476,#339),#387,.F.);
#2253=ADVANCED_FACE('',(#477),#388,.T.);
#2254=ADVANCED_FACE('',(#478),#231,.T.);
#2255=ADVANCED_FACE('',(#479),#2187,.T.);
#2256=ADVANCED_FACE('',(#480),#232,.T.);
#2257=ADVANCED_FACE('',(#481,#340),#389,.T.);
#2258=ADVANCED_FACE('',(#482),#233,.T.);
#2259=ADVANCED_FACE('',(#483),#2188,.T.);
#2260=ADVANCED_FACE('',(#484),#234,.T.);
#2261=ADVANCED_FACE('',(#485),#390,.T.);
#2262=ADVANCED_FACE('',(#486),#391,.F.);
#2263=ADVANCED_FACE('',(#487),#392,.F.);
#2264=ADVANCED_FACE('',(#488),#393,.F.);
#2265=ADVANCED_FACE('',(#489),#394,.F.);
#2266=ADVANCED_FACE('',(#490),#395,.F.);
#2267=ADVANCED_FACE('',(#491),#396,.F.);
#2268=ADVANCED_FACE('',(#492),#397,.F.);
#2269=ADVANCED_FACE('',(#493),#398,.F.);
#2270=ADVANCED_FACE('',(#494),#2189,.F.);
#2271=ADVANCED_FACE('',(#495),#399,.F.);
#2272=ADVANCED_FACE('',(#496,#341),#400,.F.);
#2273=ADVANCED_FACE('',(#497),#2190,.T.);
#2274=ADVANCED_FACE('',(#498),#401,.T.);
#2275=ADVANCED_FACE('',(#499),#2191,.T.);
#2276=ADVANCED_FACE('',(#500,#342),#402,.F.);
#2277=ADVANCED_FACE('',(#501),#2192,.F.);
#2278=ADVANCED_FACE('',(#502),#2193,.T.);
#2279=ADVANCED_FACE('',(#503,#343),#403,.T.);
#2280=ADVANCED_FACE('',(#504,#344),#404,.F.);
#2281=ADVANCED_FACE('',(#505),#2194,.F.);
#2282=ADVANCED_FACE('',(#506),#2195,.T.);
#2283=ADVANCED_FACE('',(#507,#345),#405,.T.);
#2284=ADVANCED_FACE('',(#508,#346),#406,.F.);
#2285=ADVANCED_FACE('',(#509),#2196,.F.);
#2286=ADVANCED_FACE('',(#510),#2197,.T.);
#2287=ADVANCED_FACE('',(#511,#347),#407,.T.);
#2288=ADVANCED_FACE('',(#512,#348),#408,.F.);
#2289=ADVANCED_FACE('',(#513),#409,.F.);
#2290=ADVANCED_FACE('',(#514),#410,.F.);
#2291=ADVANCED_FACE('',(#515),#411,.F.);
#2292=ADVANCED_FACE('',(#516),#412,.F.);
#2293=ADVANCED_FACE('',(#517),#413,.F.);
#2294=ADVANCED_FACE('',(#518),#414,.F.);
#2295=ADVANCED_FACE('',(#519),#415,.F.);
#2296=ADVANCED_FACE('',(#520),#416,.F.);
#2297=ADVANCED_FACE('',(#521),#417,.F.);
#2298=ADVANCED_FACE('',(#522),#418,.T.);
#2299=ADVANCED_FACE('',(#523),#235,.T.);
#2300=ADVANCED_FACE('',(#524),#2198,.T.);
#2301=ADVANCED_FACE('',(#525),#236,.T.);
#2302=ADVANCED_FACE('',(#526,#349),#419,.T.);
#2303=ADVANCED_FACE('',(#527),#237,.T.);
#2304=ADVANCED_FACE('',(#528),#2199,.T.);
#2305=ADVANCED_FACE('',(#529),#2200,.F.);
#2306=ADVANCED_FACE('',(#530,#350),#420,.T.);
#2307=ADVANCED_FACE('',(#531),#2201,.F.);
#2308=ADVANCED_FACE('',(#532,#351),#421,.F.);
#2309=ADVANCED_FACE('',(#533),#2202,.F.);
#2310=ADVANCED_FACE('',(#534),#2203,.T.);
#2311=ADVANCED_FACE('',(#535,#352),#422,.T.);
#2312=ADVANCED_FACE('',(#536,#353),#423,.F.);
#2313=ADVANCED_FACE('',(#537),#39,.F.);
#2314=ADVANCED_FACE('',(#538),#2204,.T.);
#2315=ADVANCED_FACE('',(#539),#2205,.F.);
#2316=ADVANCED_FACE('',(#540),#238,.F.);
#2317=ADVANCED_FACE('',(#541,#354),#424,.T.);
#2318=ADVANCED_FACE('',(#542),#2206,.T.);
#2319=ADVANCED_FACE('',(#543,#355),#425,.T.);
#2320=ADVANCED_FACE('',(#544),#239,.F.);
#2321=ADVANCED_FACE('',(#545),#40,.F.);
#2322=ADVANCED_FACE('',(#546),#2207,.F.);
#2323=ADVANCED_FACE('',(#547,#356),#426,.T.);
#2324=ADVANCED_FACE('',(#548),#240,.T.);
#2325=ADVANCED_FACE('',(#549),#2208,.T.);
#2326=ADVANCED_FACE('',(#550),#241,.T.);
#2327=ADVANCED_FACE('',(#551,#357),#427,.T.);
#2328=ADVANCED_FACE('',(#552),#2209,.F.);
#2329=ADVANCED_FACE('',(#553),#25,.T.);
#2330=ADVANCED_FACE('',(#554),#26,.T.);
#2331=ADVANCED_FACE('',(#555),#27,.T.);
#2332=ADVANCED_FACE('',(#556),#28,.T.);
#2333=ADVANCED_FACE('',(#557),#29,.T.);
#2334=ADVANCED_FACE('',(#558),#30,.T.);
#2335=ADVANCED_FACE('',(#559),#31,.T.);
#2336=ADVANCED_FACE('',(#560),#32,.F.);
#2337=ADVANCED_FACE('',(#561),#2210,.T.);
#2338=ADVANCED_FACE('',(#562),#428,.T.);
#2339=ADVANCED_FACE('',(#563),#33,.F.);
#2340=ADVANCED_FACE('',(#564),#429,.T.);
#2341=ADVANCED_FACE('',(#565),#34,.F.);
#2342=ADVANCED_FACE('',(#566),#430,.T.);
#2343=ADVANCED_FACE('',(#567),#35,.F.);
#2344=ADVANCED_FACE('',(#568),#431,.T.);
#2345=ADVANCED_FACE('',(#569),#36,.F.);
#2346=ADVANCED_FACE('',(#570),#432,.T.);
#2347=ADVANCED_FACE('',(#571),#37,.F.);
#2348=ADVANCED_FACE('',(#572),#2211,.F.);
#2349=ADVANCED_FACE('',(#573),#433,.T.);
#2350=ADVANCED_FACE('',(#574),#38,.F.);
#2351=ADVANCED_FACE('',(#575,#358),#434,.T.);
#2352=ADVANCED_FACE('',(#576),#435,.T.);
#2353=ADVANCED_FACE('',(#577,#359),#436,.T.);
#2354=ADVANCED_FACE('',(#578),#2212,.T.);
#2355=ADVANCED_FACE('',(#579,#360),#437,.T.);
#2356=ADVANCED_FACE('',(#580),#2213,.F.);
#2357=ADVANCED_FACE('',(#581,#361),#438,.T.);
#2358=ADVANCED_FACE('',(#582),#2214,.T.);
#2359=ADVANCED_FACE('',(#583,#362),#439,.T.);
#2360=ADVANCED_FACE('',(#584),#2215,.F.);
#2361=ADVANCED_FACE('',(#585),#2216,.F.);
#2362=ADVANCED_FACE('',(#586),#2217,.T.);
#2363=ADVANCED_FACE('',(#587,#363),#440,.T.);
#2364=ADVANCED_FACE('',(#588,#364),#441,.F.);
#2365=CLOSED_SHELL('',(#2218,#2219,#2220,#2221,#2222,#2223,#2224,#2225,
#2226,#2227,#2228,#2229,#2230,#2231));
#2366=CLOSED_SHELL('',(#2232,#2233,#2234,#2235,#2236,#2237,#2238,#2239,
#2240,#2241));
#2367=CLOSED_SHELL('',(#2242,#2243,#2244,#2245,#2246,#2247,#2248));
#2368=CLOSED_SHELL('',(#2249,#2250,#2251,#2252));
#2369=CLOSED_SHELL('',(#2253,#2254,#2255,#2256,#2257,#2258,#2259,#2260,
#2261));
#2370=CLOSED_SHELL('',(#2262,#2263,#2264,#2265,#2266,#2267,#2268,#2269));
#2371=CLOSED_SHELL('',(#2270,#2271,#2272,#2273,#2274,#2275,#2276));
#2372=CLOSED_SHELL('',(#2277,#2278,#2279,#2280));
#2373=CLOSED_SHELL('',(#2281,#2282,#2283,#2284));
#2374=CLOSED_SHELL('',(#2285,#2286,#2287,#2288));
#2375=CLOSED_SHELL('',(#2289,#2290,#2291,#2292,#2293,#2294,#2295,#2296));
#2376=CLOSED_SHELL('',(#2297,#2298,#2299,#2300,#2301,#2302,#2303,#2304));
#2377=CLOSED_SHELL('',(#2305,#2306,#2307,#2308,#2309,#2310,#2311,#2312));
#2378=CLOSED_SHELL('',(#2313,#2314,#2315,#2316,#2317,#2318,#2319,#2320));
#2379=CLOSED_SHELL('',(#2321,#2322,#2323,#2324,#2325,#2326,#2327,#2328));
#2380=CLOSED_SHELL('',(#2329));
#2381=CLOSED_SHELL('',(#2330));
#2382=CLOSED_SHELL('',(#2331));
#2383=CLOSED_SHELL('',(#2332));
#2384=CLOSED_SHELL('',(#2333));
#2385=CLOSED_SHELL('',(#2334));
#2386=CLOSED_SHELL('',(#2335));
#2387=CLOSED_SHELL('',(#2336,#2337,#2338,#2339,#2340,#2341,#2342,#2343,
#2344,#2345,#2346,#2347,#2348,#2349,#2350,#2351,#2352));
#2388=CLOSED_SHELL('',(#2353,#2354,#2355,#2356));
#2389=CLOSED_SHELL('',(#2357,#2358,#2359,#2360));
#2390=CLOSED_SHELL('',(#2361,#2362,#2363,#2364));
#2391=DERIVED_UNIT_ELEMENT(#2425,1.);
#2392=DERIVED_UNIT_ELEMENT(#4779,-3.);
#2393=DERIVED_UNIT_ELEMENT(#2425,1.);
#2394=DERIVED_UNIT_ELEMENT(#4779,-3.);
#2395=DERIVED_UNIT_ELEMENT(#2425,1.);
#2396=DERIVED_UNIT_ELEMENT(#4779,-3.);
#2397=DERIVED_UNIT_ELEMENT(#2425,1.);
#2398=DERIVED_UNIT_ELEMENT(#4779,-3.);
#2399=DERIVED_UNIT_ELEMENT(#2425,1.);
#2400=DERIVED_UNIT_ELEMENT(#4779,-3.);
#2401=DERIVED_UNIT_ELEMENT(#2425,1.);
#2402=DERIVED_UNIT_ELEMENT(#4779,-3.);
#2403=DERIVED_UNIT_ELEMENT(#2425,1.);
#2404=DERIVED_UNIT_ELEMENT(#4779,-3.);
#2405=DERIVED_UNIT_ELEMENT(#2425,1.);
#2406=DERIVED_UNIT_ELEMENT(#4779,-3.);
#2407=DERIVED_UNIT_ELEMENT(#2425,1.);
#2408=DERIVED_UNIT_ELEMENT(#4779,-3.);
#2409=DERIVED_UNIT_ELEMENT(#2425,1.);
#2410=DERIVED_UNIT_ELEMENT(#4779,-3.);
#2411=DERIVED_UNIT_ELEMENT(#2425,1.);
#2412=DERIVED_UNIT_ELEMENT(#4779,-3.);
#2413=DERIVED_UNIT_ELEMENT(#2425,1.);
#2414=DERIVED_UNIT_ELEMENT(#4779,-3.);
#2415=DERIVED_UNIT_ELEMENT(#2425,1.);
#2416=DERIVED_UNIT_ELEMENT(#4779,-3.);
#2417=DERIVED_UNIT_ELEMENT(#2425,1.);
#2418=DERIVED_UNIT_ELEMENT(#4779,-3.);
#2419=DERIVED_UNIT_ELEMENT(#2425,1.);
#2420=DERIVED_UNIT_ELEMENT(#4779,-3.);
#2421=DERIVED_UNIT_ELEMENT(#2425,1.);
#2422=DERIVED_UNIT_ELEMENT(#4779,-3.);
#2423=DERIVED_UNIT_ELEMENT(#2425,1.);
#2424=DERIVED_UNIT_ELEMENT(#4779,-3.);
#2425=(
MASS_UNIT()
NAMED_UNIT(*)
SI_UNIT(.KILO.,.GRAM.)
);
#2426=DERIVED_UNIT((#2391,#2392));
#2427=DERIVED_UNIT((#2393,#2394));
#2428=DERIVED_UNIT((#2395,#2396));
#2429=DERIVED_UNIT((#2397,#2398));
#2430=DERIVED_UNIT((#2399,#2400));
#2431=DERIVED_UNIT((#2401,#2402));
#2432=DERIVED_UNIT((#2403,#2404));
#2433=DERIVED_UNIT((#2405,#2406));
#2434=DERIVED_UNIT((#2407,#2408));
#2435=DERIVED_UNIT((#2409,#2410));
#2436=DERIVED_UNIT((#2411,#2412));
#2437=DERIVED_UNIT((#2413,#2414));
#2438=DERIVED_UNIT((#2415,#2416));
#2439=DERIVED_UNIT((#2417,#2418));
#2440=DERIVED_UNIT((#2419,#2420));
#2441=DERIVED_UNIT((#2421,#2422));
#2442=DERIVED_UNIT((#2423,#2424));
#2443=MEASURE_REPRESENTATION_ITEM('density measure',
POSITIVE_RATIO_MEASURE(7850.),#2426);
#2444=MEASURE_REPRESENTATION_ITEM('density measure',
POSITIVE_RATIO_MEASURE(7850.),#2427);
#2445=MEASURE_REPRESENTATION_ITEM('density measure',
POSITIVE_RATIO_MEASURE(7850.),#2428);
#2446=MEASURE_REPRESENTATION_ITEM('density measure',
POSITIVE_RATIO_MEASURE(7850.),#2429);
#2447=MEASURE_REPRESENTATION_ITEM('density measure',
POSITIVE_RATIO_MEASURE(7850.),#2430);
#2448=MEASURE_REPRESENTATION_ITEM('density measure',
POSITIVE_RATIO_MEASURE(7850.),#2431);
#2449=MEASURE_REPRESENTATION_ITEM('density measure',
POSITIVE_RATIO_MEASURE(7850.),#2432);
#2450=MEASURE_REPRESENTATION_ITEM('density measure',
POSITIVE_RATIO_MEASURE(7850.),#2433);
#2451=MEASURE_REPRESENTATION_ITEM('density measure',
POSITIVE_RATIO_MEASURE(7850.),#2434);
#2452=MEASURE_REPRESENTATION_ITEM('density measure',
POSITIVE_RATIO_MEASURE(7850.),#2435);
#2453=MEASURE_REPRESENTATION_ITEM('density measure',
POSITIVE_RATIO_MEASURE(7850.),#2436);
#2454=MEASURE_REPRESENTATION_ITEM('density measure',
POSITIVE_RATIO_MEASURE(7850.),#2437);
#2455=MEASURE_REPRESENTATION_ITEM('density measure',
POSITIVE_RATIO_MEASURE(7850.),#2438);
#2456=MEASURE_REPRESENTATION_ITEM('density measure',
POSITIVE_RATIO_MEASURE(7850.),#2439);
#2457=MEASURE_REPRESENTATION_ITEM('density measure',
POSITIVE_RATIO_MEASURE(7850.),#2440);
#2458=MEASURE_REPRESENTATION_ITEM('density measure',
POSITIVE_RATIO_MEASURE(7850.),#2441);
#2459=MEASURE_REPRESENTATION_ITEM('density measure',
POSITIVE_RATIO_MEASURE(7850.),#2442);
#2460=PROPERTY_DEFINITION_REPRESENTATION(#2545,#2494);
#2461=PROPERTY_DEFINITION_REPRESENTATION(#2546,#2495);
#2462=PROPERTY_DEFINITION_REPRESENTATION(#2547,#2496);
#2463=PROPERTY_DEFINITION_REPRESENTATION(#2548,#2497);
#2464=PROPERTY_DEFINITION_REPRESENTATION(#2549,#2498);
#2465=PROPERTY_DEFINITION_REPRESENTATION(#2550,#2499);
#2466=PROPERTY_DEFINITION_REPRESENTATION(#2551,#2500);
#2467=PROPERTY_DEFINITION_REPRESENTATION(#2552,#2501);
#2468=PROPERTY_DEFINITION_REPRESENTATION(#2553,#2502);
#2469=PROPERTY_DEFINITION_REPRESENTATION(#2554,#2503);
#2470=PROPERTY_DEFINITION_REPRESENTATION(#2555,#2504);
#2471=PROPERTY_DEFINITION_REPRESENTATION(#2556,#2505);
#2472=PROPERTY_DEFINITION_REPRESENTATION(#2557,#2506);
#2473=PROPERTY_DEFINITION_REPRESENTATION(#2558,#2507);
#2474=PROPERTY_DEFINITION_REPRESENTATION(#2559,#2508);
#2475=PROPERTY_DEFINITION_REPRESENTATION(#2560,#2509);
#2476=PROPERTY_DEFINITION_REPRESENTATION(#2561,#2510);
#2477=PROPERTY_DEFINITION_REPRESENTATION(#2562,#2511);
#2478=PROPERTY_DEFINITION_REPRESENTATION(#2563,#2512);
#2479=PROPERTY_DEFINITION_REPRESENTATION(#2564,#2513);
#2480=PROPERTY_DEFINITION_REPRESENTATION(#2565,#2514);
#2481=PROPERTY_DEFINITION_REPRESENTATION(#2566,#2515);
#2482=PROPERTY_DEFINITION_REPRESENTATION(#2567,#2516);
#2483=PROPERTY_DEFINITION_REPRESENTATION(#2568,#2517);
#2484=PROPERTY_DEFINITION_REPRESENTATION(#2569,#2518);
#2485=PROPERTY_DEFINITION_REPRESENTATION(#2570,#2519);
#2486=PROPERTY_DEFINITION_REPRESENTATION(#2571,#2520);
#2487=PROPERTY_DEFINITION_REPRESENTATION(#2572,#2521);
#2488=PROPERTY_DEFINITION_REPRESENTATION(#2573,#2522);
#2489=PROPERTY_DEFINITION_REPRESENTATION(#2574,#2523);
#2490=PROPERTY_DEFINITION_REPRESENTATION(#2575,#2524);
#2491=PROPERTY_DEFINITION_REPRESENTATION(#2576,#2525);
#2492=PROPERTY_DEFINITION_REPRESENTATION(#2577,#2526);
#2493=PROPERTY_DEFINITION_REPRESENTATION(#2578,#2527);
#2494=REPRESENTATION('material name',(#2528),#4758);
#2495=REPRESENTATION('density',(#2443),#4758);
#2496=REPRESENTATION('material name',(#2529),#4759);
#2497=REPRESENTATION('density',(#2444),#4759);
#2498=REPRESENTATION('material name',(#2530),#4760);
#2499=REPRESENTATION('density',(#2445),#4760);
#2500=REPRESENTATION('material name',(#2531),#4761);
#2501=REPRESENTATION('density',(#2446),#4761);
#2502=REPRESENTATION('material name',(#2532),#4762);
#2503=REPRESENTATION('density',(#2447),#4762);
#2504=REPRESENTATION('material name',(#2533),#4763);
#2505=REPRESENTATION('density',(#2448),#4763);
#2506=REPRESENTATION('material name',(#2534),#4764);
#2507=REPRESENTATION('density',(#2449),#4764);
#2508=REPRESENTATION('material name',(#2535),#4765);
#2509=REPRESENTATION('density',(#2450),#4765);
#2510=REPRESENTATION('material name',(#2536),#4766);
#2511=REPRESENTATION('density',(#2451),#4766);
#2512=REPRESENTATION('material name',(#2537),#4767);
#2513=REPRESENTATION('density',(#2452),#4767);
#2514=REPRESENTATION('material name',(#2538),#4769);
#2515=REPRESENTATION('density',(#2453),#4769);
#2516=REPRESENTATION('material name',(#2539),#4771);
#2517=REPRESENTATION('density',(#2454),#4771);
#2518=REPRESENTATION('material name',(#2540),#4772);
#2519=REPRESENTATION('density',(#2455),#4772);
#2520=REPRESENTATION('material name',(#2541),#4773);
#2521=REPRESENTATION('density',(#2456),#4773);
#2522=REPRESENTATION('material name',(#2542),#4774);
#2523=REPRESENTATION('density',(#2457),#4774);
#2524=REPRESENTATION('material name',(#2543),#4775);
#2525=REPRESENTATION('density',(#2458),#4775);
#2526=REPRESENTATION('material name',(#2544),#4776);
#2527=REPRESENTATION('density',(#2459),#4776);
#2528=DESCRIPTIVE_REPRESENTATION_ITEM('Steel','Steel');
#2529=DESCRIPTIVE_REPRESENTATION_ITEM('Steel','Steel');
#2530=DESCRIPTIVE_REPRESENTATION_ITEM('Steel','Steel');
#2531=DESCRIPTIVE_REPRESENTATION_ITEM('Steel','Steel');
#2532=DESCRIPTIVE_REPRESENTATION_ITEM('Steel','Steel');
#2533=DESCRIPTIVE_REPRESENTATION_ITEM('Steel','Steel');
#2534=DESCRIPTIVE_REPRESENTATION_ITEM('Steel','Steel');
#2535=DESCRIPTIVE_REPRESENTATION_ITEM('Steel','Steel');
#2536=DESCRIPTIVE_REPRESENTATION_ITEM('Steel','Steel');
#2537=DESCRIPTIVE_REPRESENTATION_ITEM('Steel','Steel');
#2538=DESCRIPTIVE_REPRESENTATION_ITEM('Steel','Steel');
#2539=DESCRIPTIVE_REPRESENTATION_ITEM('Steel','Steel');
#2540=DESCRIPTIVE_REPRESENTATION_ITEM('Steel','Steel');
#2541=DESCRIPTIVE_REPRESENTATION_ITEM('Steel','Steel');
#2542=DESCRIPTIVE_REPRESENTATION_ITEM('Steel','Steel');
#2543=DESCRIPTIVE_REPRESENTATION_ITEM('Steel','Steel');
#2544=DESCRIPTIVE_REPRESENTATION_ITEM('Steel','Steel');
#2545=PROPERTY_DEFINITION('material property','material name',#4895);
#2546=PROPERTY_DEFINITION('material property','density of part',#4895);
#2547=PROPERTY_DEFINITION('material property','material name',#4896);
#2548=PROPERTY_DEFINITION('material property','density of part',#4896);
#2549=PROPERTY_DEFINITION('material property','material name',#4897);
#2550=PROPERTY_DEFINITION('material property','density of part',#4897);
#2551=PROPERTY_DEFINITION('material property','material name',#4898);
#2552=PROPERTY_DEFINITION('material property','density of part',#4898);
#2553=PROPERTY_DEFINITION('material property','material name',#4899);
#2554=PROPERTY_DEFINITION('material property','density of part',#4899);
#2555=PROPERTY_DEFINITION('material property','material name',#4900);
#2556=PROPERTY_DEFINITION('material property','density of part',#4900);
#2557=PROPERTY_DEFINITION('material property','material name',#4901);
#2558=PROPERTY_DEFINITION('material property','density of part',#4901);
#2559=PROPERTY_DEFINITION('material property','material name',#4902);
#2560=PROPERTY_DEFINITION('material property','density of part',#4902);
#2561=PROPERTY_DEFINITION('material property','material name',#4903);
#2562=PROPERTY_DEFINITION('material property','density of part',#4903);
#2563=PROPERTY_DEFINITION('material property','material name',#4904);
#2564=PROPERTY_DEFINITION('material property','density of part',#4904);
#2565=PROPERTY_DEFINITION('material property','material name',#4906);
#2566=PROPERTY_DEFINITION('material property','density of part',#4906);
#2567=PROPERTY_DEFINITION('material property','material name',#4908);
#2568=PROPERTY_DEFINITION('material property','density of part',#4908);
#2569=PROPERTY_DEFINITION('material property','material name',#4909);
#2570=PROPERTY_DEFINITION('material property','density of part',#4909);
#2571=PROPERTY_DEFINITION('material property','material name',#4910);
#2572=PROPERTY_DEFINITION('material property','density of part',#4910);
#2573=PROPERTY_DEFINITION('material property','material name',#4911);
#2574=PROPERTY_DEFINITION('material property','density of part',#4911);
#2575=PROPERTY_DEFINITION('material property','material name',#4912);
#2576=PROPERTY_DEFINITION('material property','density of part',#4912);
#2577=PROPERTY_DEFINITION('material property','material name',#4913);
#2578=PROPERTY_DEFINITION('material property','density of part',#4913);
#2579=AXIS2_PLACEMENT_3D('',#3761,#2932,#2933);
#2580=AXIS2_PLACEMENT_3D('',#3762,#2934,#2935);
#2581=AXIS2_PLACEMENT_3D('',#3763,#2936,#2937);
#2582=AXIS2_PLACEMENT_3D('',#3764,#2938,#2939);
#2583=AXIS2_PLACEMENT_3D('',#3766,#2940,#2941);
#2584=AXIS2_PLACEMENT_3D('',#3769,#2943,#2944);
#2585=AXIS2_PLACEMENT_3D('',#3770,#2945,#2946);
#2586=AXIS2_PLACEMENT_3D('',#3771,#2947,#2948);
#2587=AXIS2_PLACEMENT_3D('',#3773,#2949,#2950);
#2588=AXIS2_PLACEMENT_3D('',#3776,#2952,#2953);
#2589=AXIS2_PLACEMENT_3D('',#3777,#2954,#2955);
#2590=AXIS2_PLACEMENT_3D('',#3778,#2956,#2957);
#2591=AXIS2_PLACEMENT_3D('',#3780,#2958,#2959);
#2592=AXIS2_PLACEMENT_3D('',#3783,#2961,#2962);
#2593=AXIS2_PLACEMENT_3D('',#3784,#2963,#2964);
#2594=AXIS2_PLACEMENT_3D('',#3785,#2965,#2966);
#2595=AXIS2_PLACEMENT_3D('',#3787,#2967,#2968);
#2596=AXIS2_PLACEMENT_3D('',#3790,#2970,#2971);
#2597=AXIS2_PLACEMENT_3D('',#3791,#2972,#2973);
#2598=AXIS2_PLACEMENT_3D('',#3792,#2974,#2975);
#2599=AXIS2_PLACEMENT_3D('',#3801,#2980,#2981);
#2600=AXIS2_PLACEMENT_3D('',#3807,#2985,#2986);
#2601=AXIS2_PLACEMENT_3D('',#3813,#2990,#2991);
#2602=AXIS2_PLACEMENT_3D('',#3816,#2994,#2995);
#2603=AXIS2_PLACEMENT_3D('',#3817,#2996,#2997);
#2604=AXIS2_PLACEMENT_3D('',#3818,#2998,#2999);
#2605=AXIS2_PLACEMENT_3D('',#3819,#3000,#3001);
#2606=AXIS2_PLACEMENT_3D('',#3821,#3002,#3003);
#2607=AXIS2_PLACEMENT_3D('',#3824,#3005,#3006);
#2608=AXIS2_PLACEMENT_3D('',#3825,#3007,#3008);
#2609=AXIS2_PLACEMENT_3D('',#3827,#3009,#3010);
#2610=AXIS2_PLACEMENT_3D('',#3830,#3012,#3013);
#2611=AXIS2_PLACEMENT_3D('',#3831,#3014,#3015);
#2612=AXIS2_PLACEMENT_3D('',#3833,#3016,#3017);
#2613=AXIS2_PLACEMENT_3D('',#3836,#3019,#3020);
#2614=AXIS2_PLACEMENT_3D('',#3837,#3021,#3022);
#2615=AXIS2_PLACEMENT_3D('',#3839,#3023,#3024);
#2616=AXIS2_PLACEMENT_3D('',#3842,#3026,#3027);
#2617=AXIS2_PLACEMENT_3D('',#3843,#3028,#3029);
#2618=AXIS2_PLACEMENT_3D('',#3852,#3034,#3035);
#2619=AXIS2_PLACEMENT_3D('',#3858,#3039,#3040);
#2620=AXIS2_PLACEMENT_3D('',#3864,#3044,#3045);
#2621=AXIS2_PLACEMENT_3D('',#3867,#3048,#3049);
#2622=AXIS2_PLACEMENT_3D('',#3868,#3050,#3051);
#2623=AXIS2_PLACEMENT_3D('',#3869,#3052,#3053);
#2624=AXIS2_PLACEMENT_3D('',#3870,#3054,#3055);
#2625=AXIS2_PLACEMENT_3D('',#3872,#3056,#3057);
#2626=AXIS2_PLACEMENT_3D('',#3875,#3059,#3060);
#2627=AXIS2_PLACEMENT_3D('',#3876,#3061,#3062);
#2628=AXIS2_PLACEMENT_3D('',#3885,#3067,#3068);
#2629=AXIS2_PLACEMENT_3D('',#3894,#3073,#3074);
#2630=AXIS2_PLACEMENT_3D('',#3897,#3077,#3078);
#2631=AXIS2_PLACEMENT_3D('',#3898,#3079,#3080);
#2632=AXIS2_PLACEMENT_3D('',#3899,#3081,#3082);
#2633=AXIS2_PLACEMENT_3D('',#3900,#3083,#3084);
#2634=AXIS2_PLACEMENT_3D('',#3901,#3085,#3086);
#2635=AXIS2_PLACEMENT_3D('',#3902,#3087,#3088);
#2636=AXIS2_PLACEMENT_3D('',#3903,#3089,#3090);
#2637=AXIS2_PLACEMENT_3D('',#3905,#3091,#3092);
#2638=AXIS2_PLACEMENT_3D('',#3908,#3094,#3095);
#2639=AXIS2_PLACEMENT_3D('',#3909,#3096,#3097);
#2640=AXIS2_PLACEMENT_3D('',#3911,#3098,#3099);
#2641=AXIS2_PLACEMENT_3D('',#3914,#3101,#3102);
#2642=AXIS2_PLACEMENT_3D('',#3915,#3103,#3104);
#2643=AXIS2_PLACEMENT_3D('',#3916,#3105,#3106);
#2644=AXIS2_PLACEMENT_3D('',#3917,#3107,#3108);
#2645=AXIS2_PLACEMENT_3D('',#3918,#3109,#3110);
#2646=AXIS2_PLACEMENT_3D('',#3920,#3111,#3112);
#2647=AXIS2_PLACEMENT_3D('',#3921,#3113,#3114);
#2648=AXIS2_PLACEMENT_3D('',#3923,#3115,#3116);
#2649=AXIS2_PLACEMENT_3D('',#3925,#3118,#3119);
#2650=AXIS2_PLACEMENT_3D('',#3927,#3120,#3121);
#2651=AXIS2_PLACEMENT_3D('',#3929,#3123,#3124);
#2652=AXIS2_PLACEMENT_3D('',#3931,#3125,#3126);
#2653=AXIS2_PLACEMENT_3D('',#3933,#3128,#3129);
#2654=AXIS2_PLACEMENT_3D('',#3935,#3130,#3131);
#2655=AXIS2_PLACEMENT_3D('',#3936,#3132,#3133);
#2656=AXIS2_PLACEMENT_3D('',#3938,#3134,#3135);
#2657=AXIS2_PLACEMENT_3D('',#3940,#3137,#3138);
#2658=AXIS2_PLACEMENT_3D('',#3942,#3139,#3140);
#2659=AXIS2_PLACEMENT_3D('',#3944,#3142,#3143);
#2660=AXIS2_PLACEMENT_3D('',#3946,#3144,#3145);
#2661=AXIS2_PLACEMENT_3D('',#3948,#3147,#3148);
#2662=AXIS2_PLACEMENT_3D('',#3949,#3149,#3150);
#2663=AXIS2_PLACEMENT_3D('',#3958,#3155,#3156);
#2664=AXIS2_PLACEMENT_3D('',#3964,#3160,#3161);
#2665=AXIS2_PLACEMENT_3D('',#3970,#3165,#3166);
#2666=AXIS2_PLACEMENT_3D('',#3976,#3170,#3171);
#2667=AXIS2_PLACEMENT_3D('',#3982,#3175,#3176);
#2668=AXIS2_PLACEMENT_3D('',#3985,#3179,#3180);
#2669=AXIS2_PLACEMENT_3D('',#3986,#3181,#3182);
#2670=AXIS2_PLACEMENT_3D('',#3987,#3183,#3184);
#2671=AXIS2_PLACEMENT_3D('',#3988,#3185,#3186);
#2672=AXIS2_PLACEMENT_3D('',#3990,#3187,#3188);
#2673=AXIS2_PLACEMENT_3D('',#3993,#3190,#3191);
#2674=AXIS2_PLACEMENT_3D('',#3994,#3192,#3193);
#2675=AXIS2_PLACEMENT_3D('',#3995,#3194,#3195);
#2676=AXIS2_PLACEMENT_3D('',#3997,#3196,#3197);
#2677=AXIS2_PLACEMENT_3D('',#3999,#3198,#3199);
#2678=AXIS2_PLACEMENT_3D('',#4000,#3200,#3201);
#2679=AXIS2_PLACEMENT_3D('',#4002,#3202,#3203);
#2680=AXIS2_PLACEMENT_3D('',#4004,#3205,#3206);
#2681=AXIS2_PLACEMENT_3D('',#4005,#3207,#3208);
#2682=AXIS2_PLACEMENT_3D('',#4008,#3210,#3211);
#2683=AXIS2_PLACEMENT_3D('',#4009,#3212,#3213);
#2684=AXIS2_PLACEMENT_3D('',#4010,#3214,#3215);
#2685=AXIS2_PLACEMENT_3D('',#4011,#3216,#3217);
#2686=AXIS2_PLACEMENT_3D('',#4013,#3218,#3219);
#2687=AXIS2_PLACEMENT_3D('',#4016,#3221,#3222);
#2688=AXIS2_PLACEMENT_3D('',#4017,#3223,#3224);
#2689=AXIS2_PLACEMENT_3D('',#4019,#3225,#3226);
#2690=AXIS2_PLACEMENT_3D('',#4022,#3228,#3229);
#2691=AXIS2_PLACEMENT_3D('',#4023,#3230,#3231);
#2692=AXIS2_PLACEMENT_3D('',#4024,#3232,#3233);
#2693=AXIS2_PLACEMENT_3D('',#4025,#3234,#3235);
#2694=AXIS2_PLACEMENT_3D('',#4026,#3236,#3237);
#2695=AXIS2_PLACEMENT_3D('',#4028,#3238,#3239);
#2696=AXIS2_PLACEMENT_3D('',#4031,#3241,#3242);
#2697=AXIS2_PLACEMENT_3D('',#4032,#3243,#3244);
#2698=AXIS2_PLACEMENT_3D('',#4034,#3245,#3246);
#2699=AXIS2_PLACEMENT_3D('',#4037,#3248,#3249);
#2700=AXIS2_PLACEMENT_3D('',#4038,#3250,#3251);
#2701=AXIS2_PLACEMENT_3D('',#4039,#3252,#3253);
#2702=AXIS2_PLACEMENT_3D('',#4040,#3254,#3255);
#2703=AXIS2_PLACEMENT_3D('',#4041,#3256,#3257);
#2704=AXIS2_PLACEMENT_3D('',#4043,#3258,#3259);
#2705=AXIS2_PLACEMENT_3D('',#4046,#3261,#3262);
#2706=AXIS2_PLACEMENT_3D('',#4047,#3263,#3264);
#2707=AXIS2_PLACEMENT_3D('',#4049,#3265,#3266);
#2708=AXIS2_PLACEMENT_3D('',#4052,#3268,#3269);
#2709=AXIS2_PLACEMENT_3D('',#4053,#3270,#3271);
#2710=AXIS2_PLACEMENT_3D('',#4054,#3272,#3273);
#2711=AXIS2_PLACEMENT_3D('',#4055,#3274,#3275);
#2712=AXIS2_PLACEMENT_3D('',#4056,#3276,#3277);
#2713=AXIS2_PLACEMENT_3D('',#4065,#3282,#3283);
#2714=AXIS2_PLACEMENT_3D('',#4071,#3287,#3288);
#2715=AXIS2_PLACEMENT_3D('',#4077,#3292,#3293);
#2716=AXIS2_PLACEMENT_3D('',#4083,#3297,#3298);
#2717=AXIS2_PLACEMENT_3D('',#4089,#3302,#3303);
#2718=AXIS2_PLACEMENT_3D('',#4092,#3306,#3307);
#2719=AXIS2_PLACEMENT_3D('',#4093,#3308,#3309);
#2720=AXIS2_PLACEMENT_3D('',#4094,#3310,#3311);
#2721=AXIS2_PLACEMENT_3D('',#4096,#3312,#3313);
#2722=AXIS2_PLACEMENT_3D('',#4097,#3314,#3315);
#2723=AXIS2_PLACEMENT_3D('',#4099,#3316,#3317);
#2724=AXIS2_PLACEMENT_3D('',#4100,#3318,#3319);
#2725=AXIS2_PLACEMENT_3D('',#4102,#3320,#3321);
#2726=AXIS2_PLACEMENT_3D('',#4104,#3323,#3324);
#2727=AXIS2_PLACEMENT_3D('',#4106,#3325,#3326);
#2728=AXIS2_PLACEMENT_3D('',#4108,#3328,#3329);
#2729=AXIS2_PLACEMENT_3D('',#4110,#3330,#3331);
#2730=AXIS2_PLACEMENT_3D('',#4112,#3333,#3334);
#2731=AXIS2_PLACEMENT_3D('',#4114,#3335,#3336);
#2732=AXIS2_PLACEMENT_3D('',#4115,#3337,#3338);
#2733=AXIS2_PLACEMENT_3D('',#4117,#3339,#3340);
#2734=AXIS2_PLACEMENT_3D('',#4119,#3342,#3343);
#2735=AXIS2_PLACEMENT_3D('',#4121,#3345,#3346);
#2736=AXIS2_PLACEMENT_3D('',#4122,#3347,#3348);
#2737=AXIS2_PLACEMENT_3D('',#4123,#3349,#3350);
#2738=AXIS2_PLACEMENT_3D('',#4124,#3351,#3352);
#2739=AXIS2_PLACEMENT_3D('',#4125,#3353,#3354);
#2740=AXIS2_PLACEMENT_3D('',#4126,#3355,#3356);
#2741=AXIS2_PLACEMENT_3D('',#4127,#3357,#3358);
#2742=AXIS2_PLACEMENT_3D('',#4128,#3359,#3360);
#2743=AXIS2_PLACEMENT_3D('',#4129,#3361,#3362);
#2744=AXIS2_PLACEMENT_3D('',#4130,#3363,#3364);
#2745=AXIS2_PLACEMENT_3D('',#4131,#3365,#3366);
#2746=AXIS2_PLACEMENT_3D('',#4132,#3367,#3368);
#2747=AXIS2_PLACEMENT_3D('',#4133,#3369,#3370);
#2748=AXIS2_PLACEMENT_3D('',#4134,#3371,#3372);
#2749=AXIS2_PLACEMENT_3D('',#4135,#3373,#3374);
#2750=AXIS2_PLACEMENT_3D('',#4136,#3375,#3376);
#2751=AXIS2_PLACEMENT_3D('',#4137,#3377,#3378);
#2752=AXIS2_PLACEMENT_3D('',#4138,#3379,#3380);
#2753=AXIS2_PLACEMENT_3D('',#4139,#3381,#3382);
#2754=AXIS2_PLACEMENT_3D('',#4140,#3383,#3384);
#2755=AXIS2_PLACEMENT_3D('',#4141,#3385,#3386);
#2756=AXIS2_PLACEMENT_3D('',#4142,#3387,#3388);
#2757=AXIS2_PLACEMENT_3D('',#4143,#3389,#3390);
#2758=AXIS2_PLACEMENT_3D('',#4144,#3391,#3392);
#2759=AXIS2_PLACEMENT_3D('',#4145,#3393,#3394);
#2760=AXIS2_PLACEMENT_3D('',#4146,#3395,#3396);
#2761=AXIS2_PLACEMENT_3D('',#4147,#3397,#3398);
#2762=AXIS2_PLACEMENT_3D('',#4148,#3399,#3400);
#2763=AXIS2_PLACEMENT_3D('',#4149,#3401,#3402);
#2764=AXIS2_PLACEMENT_3D('',#4150,#3403,#3404);
#2765=AXIS2_PLACEMENT_3D('',#4151,#3405,#3406);
#2766=AXIS2_PLACEMENT_3D('',#4152,#3407,#3408);
#2767=AXIS2_PLACEMENT_3D('',#4153,#3409,#3410);
#2768=AXIS2_PLACEMENT_3D('',#4154,#3411,#3412);
#2769=AXIS2_PLACEMENT_3D('',#4155,#3413,#3414);
#2770=AXIS2_PLACEMENT_3D('',#4157,#3415,#3416);
#2771=AXIS2_PLACEMENT_3D('',#4160,#3418,#3419);
#2772=AXIS2_PLACEMENT_3D('',#4161,#3420,#3421);
#2773=AXIS2_PLACEMENT_3D('',#4163,#3422,#3423);
#2774=AXIS2_PLACEMENT_3D('',#4164,#3424,#3425);
#2775=AXIS2_PLACEMENT_3D('',#4166,#3426,#3427);
#2776=AXIS2_PLACEMENT_3D('',#4169,#3429,#3430);
#2777=AXIS2_PLACEMENT_3D('',#4170,#3431,#3432);
#2778=AXIS2_PLACEMENT_3D('',#4172,#3433,#3434);
#2779=AXIS2_PLACEMENT_3D('',#4173,#3435,#3436);
#2780=AXIS2_PLACEMENT_3D('',#4175,#3438,#3439);
#2781=AXIS2_PLACEMENT_3D('',#4177,#3440,#3441);
#2782=AXIS2_PLACEMENT_3D('',#4180,#3443,#3444);
#2783=AXIS2_PLACEMENT_3D('',#4181,#3445,#3446);
#2784=AXIS2_PLACEMENT_3D('',#4182,#3447,#3448);
#2785=AXIS2_PLACEMENT_3D('',#4183,#3449,#3450);
#2786=AXIS2_PLACEMENT_3D('',#4184,#3451,#3452);
#2787=AXIS2_PLACEMENT_3D('',#4185,#3453,#3454);
#2788=AXIS2_PLACEMENT_3D('',#4188,#3455,#3456);
#2789=AXIS2_PLACEMENT_3D('',#4189,#3457,#3458);
#2790=AXIS2_PLACEMENT_3D('',#4191,#3459,#3460);
#2791=AXIS2_PLACEMENT_3D('',#4193,#3461,#3462);
#2792=AXIS2_PLACEMENT_3D('',#4194,#3463,#3464);
#2793=AXIS2_PLACEMENT_3D('',#4195,#3465,#3466);
#2794=AXIS2_PLACEMENT_3D('',#4198,#3468,#3469);
#2795=AXIS2_PLACEMENT_3D('',#4199,#3470,#3471);
#2796=AXIS2_PLACEMENT_3D('',#4201,#3472,#3473);
#2797=AXIS2_PLACEMENT_3D('',#4204,#3475,#3476);
#2798=AXIS2_PLACEMENT_3D('',#4205,#3477,#3478);
#2799=AXIS2_PLACEMENT_3D('',#4208,#3480,#3481);
#2800=AXIS2_PLACEMENT_3D('',#4209,#3482,#3483);
#2801=AXIS2_PLACEMENT_3D('',#4210,#3484,#3485);
#2802=AXIS2_PLACEMENT_3D('',#4212,#3486,#3487);
#2803=AXIS2_PLACEMENT_3D('',#4214,#3489,#3490);
#2804=AXIS2_PLACEMENT_3D('',#4216,#3491,#3492);
#2805=AXIS2_PLACEMENT_3D('',#4217,#3493,#3494);
#2806=AXIS2_PLACEMENT_3D('',#4219,#3496,#3497);
#2807=AXIS2_PLACEMENT_3D('',#4220,#3498,#3499);
#2808=AXIS2_PLACEMENT_3D('',#4223,#3500,#3501);
#2809=AXIS2_PLACEMENT_3D('',#4224,#3502,#3503);
#2810=AXIS2_PLACEMENT_3D('',#4226,#3504,#3505);
#2811=AXIS2_PLACEMENT_3D('',#4228,#3506,#3507);
#2812=AXIS2_PLACEMENT_3D('',#4229,#3508,#3509);
#2813=AXIS2_PLACEMENT_3D('',#4230,#3510,#3511);
#2814=AXIS2_PLACEMENT_3D('',#4232,#3512,#3513);
#2815=AXIS2_PLACEMENT_3D('',#4234,#3515,#3516);
#2816=AXIS2_PLACEMENT_3D('',#4236,#3517,#3518);
#2817=AXIS2_PLACEMENT_3D('',#4238,#3519,#3520);
#2818=AXIS2_PLACEMENT_3D('',#4239,#3521,#3522);
#2819=AXIS2_PLACEMENT_3D('',#4241,#3523,#3524);
#2820=AXIS2_PLACEMENT_3D('',#4243,#3526,#3527);
#2821=AXIS2_PLACEMENT_3D('',#4245,#3528,#3529);
#2822=AXIS2_PLACEMENT_3D('',#4247,#3531,#3532);
#2823=AXIS2_PLACEMENT_3D('',#4249,#3533,#3534);
#2824=AXIS2_PLACEMENT_3D('',#4251,#3536,#3537);
#2825=AXIS2_PLACEMENT_3D('',#4252,#3538,#3539);
#2826=AXIS2_PLACEMENT_3D('',#4254,#3541,#3542);
#2827=AXIS2_PLACEMENT_3D('',#4255,#3543,#3544);
#2828=AXIS2_PLACEMENT_3D('',#4258,#3545,#3546);
#2829=AXIS2_PLACEMENT_3D('',#4259,#3547,#3548);
#2830=AXIS2_PLACEMENT_3D('',#4262,#3549,#3550);
#2831=AXIS2_PLACEMENT_3D('',#4263,#3551,#3552);
#2832=AXIS2_PLACEMENT_3D('',#4266,#3553,#3554);
#2833=AXIS2_PLACEMENT_3D('',#4267,#3555,#3556);
#2834=AXIS2_PLACEMENT_3D('',#4270,#3557,#3558);
#2835=AXIS2_PLACEMENT_3D('',#4271,#3559,#3560);
#2836=AXIS2_PLACEMENT_3D('',#4274,#3561,#3562);
#2837=AXIS2_PLACEMENT_3D('',#4275,#3563,#3564);
#2838=AXIS2_PLACEMENT_3D('',#4278,#3565,#3566);
#2839=AXIS2_PLACEMENT_3D('',#4279,#3567,#3568);
#2840=AXIS2_PLACEMENT_3D('',#4282,#3569,#3570);
#2841=AXIS2_PLACEMENT_3D('',#4283,#3571,#3572);
#2842=AXIS2_PLACEMENT_3D('',#4284,#3573,#3574);
#2843=AXIS2_PLACEMENT_3D('',#4310,#3575,#3576);
#2844=AXIS2_PLACEMENT_3D('',#4334,#3577,#3578);
#2845=AXIS2_PLACEMENT_3D('',#4335,#3579,#3580);
#2846=AXIS2_PLACEMENT_3D('',#4337,#3581,#3582);
#2847=AXIS2_PLACEMENT_3D('',#4362,#3583,#3584);
#2848=AXIS2_PLACEMENT_3D('',#4387,#3585,#3586);
#2849=AXIS2_PLACEMENT_3D('',#4390,#3588,#3589);
#2850=AXIS2_PLACEMENT_3D('',#4392,#3590,#3591);
#2851=AXIS2_PLACEMENT_3D('',#4417,#3592,#3593);
#2852=AXIS2_PLACEMENT_3D('',#4442,#3594,#3595);
#2853=AXIS2_PLACEMENT_3D('',#4467,#3596,#3597);
#2854=AXIS2_PLACEMENT_3D('',#4491,#3598,#3599);
#2855=AXIS2_PLACEMENT_3D('',#4492,#3600,#3601);
#2856=AXIS2_PLACEMENT_3D('',#4494,#3602,#3603);
#2857=AXIS2_PLACEMENT_3D('',#4495,#3604,#3605);
#2858=AXIS2_PLACEMENT_3D('',#4496,#3606,#3607);
#2859=AXIS2_PLACEMENT_3D('',#4520,#3608,#3609);
#2860=AXIS2_PLACEMENT_3D('',#4521,#3610,#3611);
#2861=AXIS2_PLACEMENT_3D('',#4523,#3612,#3613);
#2862=AXIS2_PLACEMENT_3D('',#4524,#3614,#3615);
#2863=AXIS2_PLACEMENT_3D('',#4525,#3616,#3617);
#2864=AXIS2_PLACEMENT_3D('',#4549,#3618,#3619);
#2865=AXIS2_PLACEMENT_3D('',#4550,#3620,#3621);
#2866=AXIS2_PLACEMENT_3D('',#4552,#3622,#3623);
#2867=AXIS2_PLACEMENT_3D('',#4554,#3624,#3625);
#2868=AXIS2_PLACEMENT_3D('',#4555,#3626,#3627);
#2869=AXIS2_PLACEMENT_3D('',#4556,#3628,#3629);
#2870=AXIS2_PLACEMENT_3D('',#4580,#3630,#3631);
#2871=AXIS2_PLACEMENT_3D('',#4581,#3632,#3633);
#2872=AXIS2_PLACEMENT_3D('',#4583,#3634,#3635);
#2873=AXIS2_PLACEMENT_3D('',#4584,#3636,#3637);
#2874=AXIS2_PLACEMENT_3D('',#4585,#3638,#3639);
#2875=AXIS2_PLACEMENT_3D('',#4609,#3640,#3641);
#2876=AXIS2_PLACEMENT_3D('',#4610,#3642,#3643);
#2877=AXIS2_PLACEMENT_3D('',#4612,#3644,#3645);
#2878=AXIS2_PLACEMENT_3D('',#4613,#3646,#3647);
#2879=AXIS2_PLACEMENT_3D('',#4614,#3648,#3649);
#2880=AXIS2_PLACEMENT_3D('',#4638,#3650,#3651);
#2881=AXIS2_PLACEMENT_3D('',#4639,#3652,#3653);
#2882=AXIS2_PLACEMENT_3D('',#4641,#3654,#3655);
#2883=AXIS2_PLACEMENT_3D('',#4644,#3657,#3658);
#2884=AXIS2_PLACEMENT_3D('',#4668,#3659,#3660);
#2885=AXIS2_PLACEMENT_3D('',#4669,#3661,#3662);
#2886=AXIS2_PLACEMENT_3D('',#4670,#3663,#3664);
#2887=AXIS2_PLACEMENT_3D('',#4671,#3665,#3666);
#2888=AXIS2_PLACEMENT_3D('',#4672,#3667,#3668);
#2889=AXIS2_PLACEMENT_3D('',#4673,#3669,#3670);
#2890=AXIS2_PLACEMENT_3D('',#4674,#3671,#3672);
#2891=AXIS2_PLACEMENT_3D('',#4675,#3673,#3674);
#2892=AXIS2_PLACEMENT_3D('',#4676,#3675,#3676);
#2893=AXIS2_PLACEMENT_3D('',#4678,#3677,#3678);
#2894=AXIS2_PLACEMENT_3D('',#4680,#3679,#3680);
#2895=AXIS2_PLACEMENT_3D('',#4681,#3681,#3682);
#2896=AXIS2_PLACEMENT_3D('',#4683,#3683,#3684);
#2897=AXIS2_PLACEMENT_3D('',#4685,#3686,#3687);
#2898=AXIS2_PLACEMENT_3D('',#4687,#3688,#3689);
#2899=AXIS2_PLACEMENT_3D('',#4688,#3690,#3691);
#2900=AXIS2_PLACEMENT_3D('',#4690,#3693,#3694);
#2901=AXIS2_PLACEMENT_3D('',#4692,#3695,#3696);
#2902=AXIS2_PLACEMENT_3D('',#4694,#3697,#3698);
#2903=AXIS2_PLACEMENT_3D('',#4695,#3699,#3700);
#2904=AXIS2_PLACEMENT_3D('',#4697,#3701,#3702);
#2905=AXIS2_PLACEMENT_3D('',#4699,#3704,#3705);
#2906=AXIS2_PLACEMENT_3D('',#4701,#3706,#3707);
#2907=AXIS2_PLACEMENT_3D('',#4702,#3708,#3709);
#2908=AXIS2_PLACEMENT_3D('',#4704,#3711,#3712);
#2909=AXIS2_PLACEMENT_3D('',#4705,#3713,#3714);
#2910=AXIS2_PLACEMENT_3D('',#4706,#3715,#3716);
#2911=AXIS2_PLACEMENT_3D('',#4707,#3717,#3718);
#2912=AXIS2_PLACEMENT_3D('',#4708,#3719,#3720);
#2913=AXIS2_PLACEMENT_3D('',#4709,#3721,#3722);
#2914=AXIS2_PLACEMENT_3D('',#4710,#3723,#3724);
#2915=AXIS2_PLACEMENT_3D('',#4712,#3725,#3726);
#2916=AXIS2_PLACEMENT_3D('',#4715,#3728,#3729);
#2917=AXIS2_PLACEMENT_3D('',#4716,#3730,#3731);
#2918=AXIS2_PLACEMENT_3D('',#4718,#3732,#3733);
#2919=AXIS2_PLACEMENT_3D('',#4721,#3735,#3736);
#2920=AXIS2_PLACEMENT_3D('',#4722,#3737,#3738);
#2921=AXIS2_PLACEMENT_3D('',#4723,#3739,#3740);
#2922=AXIS2_PLACEMENT_3D('',#4724,#3741,#3742);
#2923=AXIS2_PLACEMENT_3D('',#4725,#3743,#3744);
#2924=AXIS2_PLACEMENT_3D('',#4726,#3745,#3746);
#2925=AXIS2_PLACEMENT_3D('',#4727,#3747,#3748);
#2926=AXIS2_PLACEMENT_3D('',#4728,#3749,#3750);
#2927=AXIS2_PLACEMENT_3D('',#4729,#3751,#3752);
#2928=AXIS2_PLACEMENT_3D('',#4730,#3753,#3754);
#2929=AXIS2_PLACEMENT_3D('',#4731,#3755,#3756);
#2930=AXIS2_PLACEMENT_3D('',#4732,#3757,#3758);
#2931=AXIS2_PLACEMENT_3D('',#4733,#3759,#3760);
#2932=DIRECTION('axis',(0.,0.,1.));
#2933=DIRECTION('refdir',(1.,0.,0.));
#2934=DIRECTION('axis',(0.,0.,1.));
#2935=DIRECTION('refdir',(1.,0.,0.));
#2936=DIRECTION('axis',(0.,0.,1.));
#2937=DIRECTION('refdir',(1.,0.,0.));
#2938=DIRECTION('center_axis',(0.,1.,0.));
#2939=DIRECTION('ref_axis',(1.,0.,0.));
#2940=DIRECTION('center_axis',(0.,1.,0.));
#2941=DIRECTION('ref_axis',(1.,0.,0.));
#2942=DIRECTION('',(0.,1.,0.));
#2943=DIRECTION('center_axis',(0.,-1.,0.));
#2944=DIRECTION('ref_axis',(1.,0.,0.));
#2945=DIRECTION('center_axis',(0.,1.,0.));
#2946=DIRECTION('ref_axis',(1.,0.,0.));
#2947=DIRECTION('center_axis',(0.,1.,0.));
#2948=DIRECTION('ref_axis',(1.,0.,0.));
#2949=DIRECTION('center_axis',(0.,1.,0.));
#2950=DIRECTION('ref_axis',(1.,0.,0.));
#2951=DIRECTION('',(0.,1.,0.));
#2952=DIRECTION('center_axis',(0.,-1.,0.));
#2953=DIRECTION('ref_axis',(1.,0.,0.));
#2954=DIRECTION('center_axis',(0.,1.,0.));
#2955=DIRECTION('ref_axis',(1.,0.,0.));
#2956=DIRECTION('center_axis',(0.,1.,0.));
#2957=DIRECTION('ref_axis',(1.,0.,0.));
#2958=DIRECTION('center_axis',(0.,1.,0.));
#2959=DIRECTION('ref_axis',(1.,0.,0.));
#2960=DIRECTION('',(0.,1.,0.));
#2961=DIRECTION('center_axis',(0.,1.,0.));
#2962=DIRECTION('ref_axis',(1.,0.,0.));
#2963=DIRECTION('center_axis',(0.,1.,0.));
#2964=DIRECTION('ref_axis',(1.,0.,0.));
#2965=DIRECTION('center_axis',(0.,1.,0.));
#2966=DIRECTION('ref_axis',(1.,0.,0.));
#2967=DIRECTION('center_axis',(0.,1.,0.));
#2968=DIRECTION('ref_axis',(1.,0.,0.));
#2969=DIRECTION('',(0.,1.,0.));
#2970=DIRECTION('center_axis',(0.,1.,0.));
#2971=DIRECTION('ref_axis',(1.,0.,0.));
#2972=DIRECTION('center_axis',(0.,1.,0.));
#2973=DIRECTION('ref_axis',(1.,0.,0.));
#2974=DIRECTION('center_axis',(0.,1.,0.));
#2975=DIRECTION('ref_axis',(-1.,0.,0.));
#2976=DIRECTION('',(-1.,0.,0.));
#2977=DIRECTION('',(0.,0.,1.));
#2978=DIRECTION('',(-1.,0.,0.));
#2979=DIRECTION('',(0.,0.,1.));
#2980=DIRECTION('center_axis',(1.,0.,0.));
#2981=DIRECTION('ref_axis',(0.,1.,0.));
#2982=DIRECTION('',(0.,1.,0.));
#2983=DIRECTION('',(0.,1.,0.));
#2984=DIRECTION('',(0.,0.,1.));
#2985=DIRECTION('center_axis',(0.,-1.,0.));
#2986=DIRECTION('ref_axis',(1.,0.,0.));
#2987=DIRECTION('',(1.,0.,0.));
#2988=DIRECTION('',(1.,0.,0.));
#2989=DIRECTION('',(0.,0.,1.));
#2990=DIRECTION('center_axis',(-1.,0.,0.));
#2991=DIRECTION('ref_axis',(0.,-1.,0.));
#2992=DIRECTION('',(0.,-1.,0.));
#2993=DIRECTION('',(0.,-1.,0.));
#2994=DIRECTION('center_axis',(0.,0.,1.));
#2995=DIRECTION('ref_axis',(1.,0.,0.));
#2996=DIRECTION('center_axis',(0.,0.,1.));
#2997=DIRECTION('ref_axis',(1.,0.,0.));
#2998=DIRECTION('axis',(0.,0.,1.));
#2999=DIRECTION('refdir',(1.,0.,0.));
#3000=DIRECTION('center_axis',(0.,1.,0.));
#3001=DIRECTION('ref_axis',(1.,0.,0.));
#3002=DIRECTION('center_axis',(0.,1.,0.));
#3003=DIRECTION('ref_axis',(1.,0.,0.));
#3004=DIRECTION('',(0.,1.,0.));
#3005=DIRECTION('center_axis',(0.,-1.,0.));
#3006=DIRECTION('ref_axis',(1.,0.,0.));
#3007=DIRECTION('center_axis',(0.,1.,0.));
#3008=DIRECTION('ref_axis',(1.,0.,0.));
#3009=DIRECTION('center_axis',(0.,1.,0.));
#3010=DIRECTION('ref_axis',(1.,0.,0.));
#3011=DIRECTION('',(0.,1.,0.));
#3012=DIRECTION('center_axis',(0.,-1.,0.));
#3013=DIRECTION('ref_axis',(1.,0.,0.));
#3014=DIRECTION('center_axis',(0.,1.,0.));
#3015=DIRECTION('ref_axis',(1.,0.,0.));
#3016=DIRECTION('center_axis',(0.,1.,0.));
#3017=DIRECTION('ref_axis',(1.,0.,0.));
#3018=DIRECTION('',(0.,1.,0.));
#3019=DIRECTION('center_axis',(0.,-1.,0.));
#3020=DIRECTION('ref_axis',(1.,0.,0.));
#3021=DIRECTION('center_axis',(0.,1.,0.));
#3022=DIRECTION('ref_axis',(1.,0.,0.));
#3023=DIRECTION('center_axis',(0.,1.,0.));
#3024=DIRECTION('ref_axis',(1.,0.,0.));
#3025=DIRECTION('',(0.,1.,0.));
#3026=DIRECTION('center_axis',(0.,-1.,0.));
#3027=DIRECTION('ref_axis',(1.,0.,0.));
#3028=DIRECTION('center_axis',(0.,1.,0.));
#3029=DIRECTION('ref_axis',(-1.,0.,0.));
#3030=DIRECTION('',(-1.,0.,0.));
#3031=DIRECTION('',(0.,0.,1.));
#3032=DIRECTION('',(-1.,0.,0.));
#3033=DIRECTION('',(0.,0.,1.));
#3034=DIRECTION('center_axis',(1.,0.,0.));
#3035=DIRECTION('ref_axis',(0.,1.,0.));
#3036=DIRECTION('',(0.,1.,0.));
#3037=DIRECTION('',(0.,1.,0.));
#3038=DIRECTION('',(0.,0.,1.));
#3039=DIRECTION('center_axis',(0.,-1.,0.));
#3040=DIRECTION('ref_axis',(1.,0.,0.));
#3041=DIRECTION('',(1.,0.,0.));
#3042=DIRECTION('',(1.,0.,0.));
#3043=DIRECTION('',(0.,0.,1.));
#3044=DIRECTION('center_axis',(-1.,0.,0.));
#3045=DIRECTION('ref_axis',(0.,-1.,0.));
#3046=DIRECTION('',(0.,-1.,0.));
#3047=DIRECTION('',(0.,-1.,0.));
#3048=DIRECTION('center_axis',(0.,0.,1.));
#3049=DIRECTION('ref_axis',(1.,0.,0.));
#3050=DIRECTION('center_axis',(0.,0.,1.));
#3051=DIRECTION('ref_axis',(1.,0.,0.));
#3052=DIRECTION('axis',(0.,0.,1.));
#3053=DIRECTION('refdir',(1.,0.,0.));
#3054=DIRECTION('center_axis',(0.,1.,0.));
#3055=DIRECTION('ref_axis',(1.,0.,0.));
#3056=DIRECTION('center_axis',(0.,1.,0.));
#3057=DIRECTION('ref_axis',(1.,0.,0.));
#3058=DIRECTION('',(0.,1.,0.));
#3059=DIRECTION('center_axis',(0.,-1.,0.));
#3060=DIRECTION('ref_axis',(1.,0.,0.));
#3061=DIRECTION('center_axis',(-1.,0.,0.));
#3062=DIRECTION('ref_axis',(0.,0.,1.));
#3063=DIRECTION('',(0.,0.,-1.));
#3064=DIRECTION('',(0.,1.,0.));
#3065=DIRECTION('',(0.,0.,1.));
#3066=DIRECTION('',(0.,1.,0.));
#3067=DIRECTION('center_axis',(1.,0.,0.));
#3068=DIRECTION('ref_axis',(0.,0.,-1.));
#3069=DIRECTION('',(0.,0.,1.));
#3070=DIRECTION('',(0.,-1.,0.));
#3071=DIRECTION('',(0.,0.,-1.));
#3072=DIRECTION('',(0.,1.,0.));
#3073=DIRECTION('center_axis',(0.,0.,1.));
#3074=DIRECTION('ref_axis',(1.,0.,0.));
#3075=DIRECTION('',(1.,0.,0.));
#3076=DIRECTION('',(-1.,0.,0.));
#3077=DIRECTION('center_axis',(0.,1.,0.));
#3078=DIRECTION('ref_axis',(1.,0.,0.));
#3079=DIRECTION('center_axis',(0.,1.,0.));
#3080=DIRECTION('ref_axis',(1.,0.,0.));
#3081=DIRECTION('center_axis',(0.,1.,0.));
#3082=DIRECTION('ref_axis',(1.,0.,0.));
#3083=DIRECTION('center_axis',(0.,1.,0.));
#3084=DIRECTION('ref_axis',(1.,0.,0.));
#3085=DIRECTION('center_axis',(0.,1.,0.));
#3086=DIRECTION('ref_axis',(1.,0.,0.));
#3087=DIRECTION('axis',(0.,0.,1.));
#3088=DIRECTION('refdir',(1.,0.,0.));
#3089=DIRECTION('center_axis',(0.,1.,0.));
#3090=DIRECTION('ref_axis',(1.,0.,0.));
#3091=DIRECTION('center_axis',(0.,-1.,0.));
#3092=DIRECTION('ref_axis',(1.,0.,0.));
#3093=DIRECTION('',(0.,-1.,0.));
#3094=DIRECTION('center_axis',(0.,-1.,0.));
#3095=DIRECTION('ref_axis',(1.,0.,0.));
#3096=DIRECTION('center_axis',(0.,1.,0.));
#3097=DIRECTION('ref_axis',(1.,0.,0.));
#3098=DIRECTION('center_axis',(0.,1.,0.));
#3099=DIRECTION('ref_axis',(1.,0.,0.));
#3100=DIRECTION('',(0.,-1.,0.));
#3101=DIRECTION('center_axis',(0.,1.,0.));
#3102=DIRECTION('ref_axis',(1.,0.,0.));
#3103=DIRECTION('center_axis',(0.,1.,0.));
#3104=DIRECTION('ref_axis',(1.,0.,0.));
#3105=DIRECTION('center_axis',(0.,1.,0.));
#3106=DIRECTION('ref_axis',(1.,0.,0.));
#3107=DIRECTION('axis',(0.,0.,1.));
#3108=DIRECTION('refdir',(1.,0.,0.));
#3109=DIRECTION('center_axis',(0.,1.,0.));
#3110=DIRECTION('ref_axis',(0.,0.,1.));
#3111=DIRECTION('center_axis',(0.,-1.,0.));
#3112=DIRECTION('ref_axis',(1.,0.,0.));
#3113=DIRECTION('center_axis',(0.,-1.,0.));
#3114=DIRECTION('ref_axis',(1.,0.,0.));
#3115=DIRECTION('center_axis',(0.,-1.,0.));
#3116=DIRECTION('ref_axis',(1.,0.,0.));
#3117=DIRECTION('',(0.707106781186548,0.707106781186547,8.65956056235493E-17));
#3118=DIRECTION('center_axis',(0.,-1.,0.));
#3119=DIRECTION('ref_axis',(1.,0.,0.));
#3120=DIRECTION('center_axis',(0.,-1.,0.));
#3121=DIRECTION('ref_axis',(1.,0.,0.));
#3122=DIRECTION('',(0.,1.,0.));
#3123=DIRECTION('center_axis',(0.,1.,0.));
#3124=DIRECTION('ref_axis',(1.,0.,0.));
#3125=DIRECTION('center_axis',(0.,-1.,0.));
#3126=DIRECTION('ref_axis',(1.,0.,0.));
#3127=DIRECTION('',(-0.707106781186548,0.707106781186547,-8.65956056235494E-17));
#3128=DIRECTION('center_axis',(0.,-1.,0.));
#3129=DIRECTION('ref_axis',(0.,0.,-1.));
#3130=DIRECTION('center_axis',(0.,-1.,0.));
#3131=DIRECTION('ref_axis',(1.,0.,0.));
#3132=DIRECTION('center_axis',(0.,1.,0.));
#3133=DIRECTION('ref_axis',(1.,0.,0.));
#3134=DIRECTION('center_axis',(0.,1.,0.));
#3135=DIRECTION('ref_axis',(1.,0.,0.));
#3136=DIRECTION('',(-0.447213595499958,0.894427190999916,-5.47678698264203E-17));
#3137=DIRECTION('center_axis',(0.,-1.,0.));
#3138=DIRECTION('ref_axis',(1.,0.,0.));
#3139=DIRECTION('center_axis',(0.,1.,0.));
#3140=DIRECTION('ref_axis',(1.,0.,0.));
#3141=DIRECTION('',(0.,1.,0.));
#3142=DIRECTION('center_axis',(0.,1.,0.));
#3143=DIRECTION('ref_axis',(1.,0.,0.));
#3144=DIRECTION('center_axis',(0.,-1.,0.));
#3145=DIRECTION('ref_axis',(1.,0.,0.));
#3146=DIRECTION('',(-0.707106781186547,0.707106781186548,-8.65956056235493E-17));
#3147=DIRECTION('center_axis',(0.,-1.,0.));
#3148=DIRECTION('ref_axis',(0.,0.,-1.));
#3149=DIRECTION('center_axis',(0.866025403784439,0.,-0.5));
#3150=DIRECTION('ref_axis',(0.5,0.,0.866025403784439));
#3151=DIRECTION('',(-0.5,0.,-0.866025403784439));
#3152=DIRECTION('',(0.,-1.,0.));
#3153=DIRECTION('',(0.5,0.,0.866025403784439));
#3154=DIRECTION('',(0.,-1.,0.));
#3155=DIRECTION('center_axis',(1.60246890531964E-16,0.,-1.));
#3156=DIRECTION('ref_axis',(1.,0.,1.60246890531964E-16));
#3157=DIRECTION('',(-1.,0.,-1.60246890531964E-16));
#3158=DIRECTION('',(0.,-1.,0.));
#3159=DIRECTION('',(1.,0.,1.60246890531964E-16));
#3160=DIRECTION('center_axis',(-0.866025403784439,0.,-0.5));
#3161=DIRECTION('ref_axis',(0.5,0.,-0.866025403784439));
#3162=DIRECTION('',(-0.5,0.,0.866025403784439));
#3163=DIRECTION('',(0.,-1.,0.));
#3164=DIRECTION('',(0.5,0.,-0.866025403784439));
#3165=DIRECTION('center_axis',(-0.866025403784439,0.,0.5));
#3166=DIRECTION('ref_axis',(-0.5,0.,-0.866025403784439));
#3167=DIRECTION('',(0.5,0.,0.866025403784439));
#3168=DIRECTION('',(0.,-1.,0.));
#3169=DIRECTION('',(-0.5,0.,-0.866025403784439));
#3170=DIRECTION('center_axis',(-1.60246890531964E-16,0.,1.));
#3171=DIRECTION('ref_axis',(-1.,0.,-1.60246890531964E-16));
#3172=DIRECTION('',(1.,0.,1.60246890531964E-16));
#3173=DIRECTION('',(0.,-1.,0.));
#3174=DIRECTION('',(-1.,0.,-1.60246890531964E-16));
#3175=DIRECTION('center_axis',(0.866025403784439,0.,0.5));
#3176=DIRECTION('ref_axis',(-0.5,0.,0.866025403784439));
#3177=DIRECTION('',(0.5,0.,-0.866025403784439));
#3178=DIRECTION('',(-0.5,0.,0.866025403784439));
#3179=DIRECTION('center_axis',(0.,1.,0.));
#3180=DIRECTION('ref_axis',(1.,0.,0.));
#3181=DIRECTION('center_axis',(0.,-1.,0.));
#3182=DIRECTION('ref_axis',(0.,0.,-1.));
#3183=DIRECTION('axis',(0.,0.,1.));
#3184=DIRECTION('refdir',(1.,0.,0.));
#3185=DIRECTION('center_axis',(0.,1.,0.));
#3186=DIRECTION('ref_axis',(1.,0.,0.));
#3187=DIRECTION('center_axis',(0.,1.,0.));
#3188=DIRECTION('ref_axis',(1.,0.,0.));
#3189=DIRECTION('',(0.,1.,0.));
#3190=DIRECTION('center_axis',(0.,1.,0.));
#3191=DIRECTION('ref_axis',(1.,0.,0.));
#3192=DIRECTION('center_axis',(0.,1.,0.));
#3193=DIRECTION('ref_axis',(1.,0.,0.));
#3194=DIRECTION('center_axis',(0.,1.,0.));
#3195=DIRECTION('ref_axis',(1.,0.,0.));
#3196=DIRECTION('center_axis',(0.,1.,0.));
#3197=DIRECTION('ref_axis',(1.,0.,0.));
#3198=DIRECTION('center_axis',(0.,1.,0.));
#3199=DIRECTION('ref_axis',(1.,0.,0.));
#3200=DIRECTION('center_axis',(0.,1.,0.));
#3201=DIRECTION('ref_axis',(1.,0.,0.));
#3202=DIRECTION('center_axis',(0.,1.,0.));
#3203=DIRECTION('ref_axis',(1.,0.,0.));
#3204=DIRECTION('',(0.,-1.,0.));
#3205=DIRECTION('center_axis',(0.,1.,0.));
#3206=DIRECTION('ref_axis',(1.,0.,0.));
#3207=DIRECTION('center_axis',(0.,1.,0.));
#3208=DIRECTION('ref_axis',(1.,0.,0.));
#3209=DIRECTION('',(0.,-1.,0.));
#3210=DIRECTION('center_axis',(0.,1.,0.));
#3211=DIRECTION('ref_axis',(1.,0.,0.));
#3212=DIRECTION('center_axis',(0.,1.,0.));
#3213=DIRECTION('ref_axis',(1.,0.,0.));
#3214=DIRECTION('axis',(0.,0.,1.));
#3215=DIRECTION('refdir',(1.,0.,0.));
#3216=DIRECTION('center_axis',(0.,1.,0.));
#3217=DIRECTION('ref_axis',(1.,0.,0.));
#3218=DIRECTION('center_axis',(0.,-1.,0.));
#3219=DIRECTION('ref_axis',(1.,0.,0.));
#3220=DIRECTION('',(0.,-1.,0.));
#3221=DIRECTION('center_axis',(0.,-1.,0.));
#3222=DIRECTION('ref_axis',(1.,0.,0.));
#3223=DIRECTION('center_axis',(0.,1.,0.));
#3224=DIRECTION('ref_axis',(1.,0.,0.));
#3225=DIRECTION('center_axis',(0.,1.,0.));
#3226=DIRECTION('ref_axis',(1.,0.,0.));
#3227=DIRECTION('',(0.,-1.,0.));
#3228=DIRECTION('center_axis',(0.,1.,0.));
#3229=DIRECTION('ref_axis',(1.,0.,0.));
#3230=DIRECTION('center_axis',(0.,1.,0.));
#3231=DIRECTION('ref_axis',(1.,0.,0.));
#3232=DIRECTION('center_axis',(0.,1.,0.));
#3233=DIRECTION('ref_axis',(1.,0.,0.));
#3234=DIRECTION('axis',(0.,0.,1.));
#3235=DIRECTION('refdir',(1.,0.,0.));
#3236=DIRECTION('center_axis',(0.,1.,0.));
#3237=DIRECTION('ref_axis',(1.,0.,0.));
#3238=DIRECTION('center_axis',(0.,-1.,0.));
#3239=DIRECTION('ref_axis',(1.,0.,0.));
#3240=DIRECTION('',(0.,-1.,0.));
#3241=DIRECTION('center_axis',(0.,-1.,0.));
#3242=DIRECTION('ref_axis',(1.,0.,0.));
#3243=DIRECTION('center_axis',(0.,1.,0.));
#3244=DIRECTION('ref_axis',(1.,0.,0.));
#3245=DIRECTION('center_axis',(0.,1.,0.));
#3246=DIRECTION('ref_axis',(1.,0.,0.));
#3247=DIRECTION('',(0.,-1.,0.));
#3248=DIRECTION('center_axis',(0.,1.,0.));
#3249=DIRECTION('ref_axis',(1.,0.,0.));
#3250=DIRECTION('center_axis',(0.,1.,0.));
#3251=DIRECTION('ref_axis',(1.,0.,0.));
#3252=DIRECTION('center_axis',(0.,1.,0.));
#3253=DIRECTION('ref_axis',(1.,0.,0.));
#3254=DIRECTION('axis',(0.,0.,1.));
#3255=DIRECTION('refdir',(1.,0.,0.));
#3256=DIRECTION('center_axis',(0.,1.,0.));
#3257=DIRECTION('ref_axis',(1.,0.,0.));
#3258=DIRECTION('center_axis',(0.,-1.,0.));
#3259=DIRECTION('ref_axis',(1.,0.,0.));
#3260=DIRECTION('',(0.,-1.,0.));
#3261=DIRECTION('center_axis',(0.,-1.,0.));
#3262=DIRECTION('ref_axis',(1.,0.,0.));
#3263=DIRECTION('center_axis',(0.,1.,0.));
#3264=DIRECTION('ref_axis',(1.,0.,0.));
#3265=DIRECTION('center_axis',(0.,1.,0.));
#3266=DIRECTION('ref_axis',(1.,0.,0.));
#3267=DIRECTION('',(0.,-1.,0.));
#3268=DIRECTION('center_axis',(0.,1.,0.));
#3269=DIRECTION('ref_axis',(1.,0.,0.));
#3270=DIRECTION('center_axis',(0.,1.,0.));
#3271=DIRECTION('ref_axis',(1.,0.,0.));
#3272=DIRECTION('center_axis',(0.,1.,0.));
#3273=DIRECTION('ref_axis',(1.,0.,0.));
#3274=DIRECTION('axis',(0.,0.,1.));
#3275=DIRECTION('refdir',(1.,0.,0.));
#3276=DIRECTION('center_axis',(0.866025403784439,0.,-0.5));
#3277=DIRECTION('ref_axis',(0.5,0.,0.866025403784439));
#3278=DIRECTION('',(-0.5,0.,-0.866025403784439));
#3279=DIRECTION('',(0.,-1.,0.));
#3280=DIRECTION('',(0.5,0.,0.866025403784439));
#3281=DIRECTION('',(0.,-1.,0.));
#3282=DIRECTION('center_axis',(1.60246890531964E-16,0.,-1.));
#3283=DIRECTION('ref_axis',(1.,0.,1.60246890531964E-16));
#3284=DIRECTION('',(-1.,0.,-1.60246890531964E-16));
#3285=DIRECTION('',(0.,-1.,0.));
#3286=DIRECTION('',(1.,0.,1.60246890531964E-16));
#3287=DIRECTION('center_axis',(-0.866025403784439,0.,-0.5));
#3288=DIRECTION('ref_axis',(0.5,0.,-0.866025403784439));
#3289=DIRECTION('',(-0.5,0.,0.866025403784439));
#3290=DIRECTION('',(0.,-1.,0.));
#3291=DIRECTION('',(0.5,0.,-0.866025403784439));
#3292=DIRECTION('center_axis',(-0.866025403784439,0.,0.5));
#3293=DIRECTION('ref_axis',(-0.5,0.,-0.866025403784439));
#3294=DIRECTION('',(0.5,0.,0.866025403784439));
#3295=DIRECTION('',(0.,-1.,0.));
#3296=DIRECTION('',(-0.5,0.,-0.866025403784439));
#3297=DIRECTION('center_axis',(-1.60246890531964E-16,0.,1.));
#3298=DIRECTION('ref_axis',(-1.,0.,-1.60246890531964E-16));
#3299=DIRECTION('',(1.,0.,1.60246890531964E-16));
#3300=DIRECTION('',(0.,-1.,0.));
#3301=DIRECTION('',(-1.,0.,-1.60246890531964E-16));
#3302=DIRECTION('center_axis',(0.866025403784439,0.,0.5));
#3303=DIRECTION('ref_axis',(-0.5,0.,0.866025403784439));
#3304=DIRECTION('',(0.5,0.,-0.866025403784439));
#3305=DIRECTION('',(-0.5,0.,0.866025403784439));
#3306=DIRECTION('center_axis',(0.,1.,0.));
#3307=DIRECTION('ref_axis',(1.,0.,0.));
#3308=DIRECTION('center_axis',(0.,-1.,0.));
#3309=DIRECTION('ref_axis',(0.,0.,-1.));
#3310=DIRECTION('center_axis',(0.,1.,0.));
#3311=DIRECTION('ref_axis',(1.,0.,0.));
#3312=DIRECTION('center_axis',(0.,1.,0.));
#3313=DIRECTION('ref_axis',(1.,0.,0.));
#3314=DIRECTION('center_axis',(0.,1.,0.));
#3315=DIRECTION('ref_axis',(0.,0.,1.));
#3316=DIRECTION('center_axis',(0.,-1.,0.));
#3317=DIRECTION('ref_axis',(1.,0.,0.));
#3318=DIRECTION('center_axis',(0.,-1.,0.));
#3319=DIRECTION('ref_axis',(1.,0.,0.));
#3320=DIRECTION('center_axis',(0.,-1.,0.));
#3321=DIRECTION('ref_axis',(1.,0.,0.));
#3322=DIRECTION('',(0.707106781186547,0.707106781186548,8.65956056235493E-17));
#3323=DIRECTION('center_axis',(0.,-1.,0.));
#3324=DIRECTION('ref_axis',(1.,0.,0.));
#3325=DIRECTION('center_axis',(0.,-1.,0.));
#3326=DIRECTION('ref_axis',(1.,0.,0.));
#3327=DIRECTION('',(0.,1.,0.));
#3328=DIRECTION('center_axis',(0.,1.,0.));
#3329=DIRECTION('ref_axis',(1.,0.,0.));
#3330=DIRECTION('center_axis',(0.,-1.,0.));
#3331=DIRECTION('ref_axis',(1.,0.,0.));
#3332=DIRECTION('',(-0.707106781186547,0.707106781186548,-8.65956056235493E-17));
#3333=DIRECTION('center_axis',(0.,-1.,0.));
#3334=DIRECTION('ref_axis',(0.,0.,-1.));
#3335=DIRECTION('center_axis',(0.,-1.,0.));
#3336=DIRECTION('ref_axis',(1.,0.,0.));
#3337=DIRECTION('center_axis',(0.,1.,0.));
#3338=DIRECTION('ref_axis',(1.,0.,0.));
#3339=DIRECTION('center_axis',(0.,1.,0.));
#3340=DIRECTION('ref_axis',(1.,0.,0.));
#3341=DIRECTION('',(-0.447213595499958,0.894427190999916,-5.47678698264203E-17));
#3342=DIRECTION('center_axis',(0.,-1.,0.));
#3343=DIRECTION('ref_axis',(1.,0.,0.));
#3344=DIRECTION('',(0.,1.,0.));
#3345=DIRECTION('',(0.,0.,1.));
#3346=DIRECTION('',(1.,0.,0.));
#3347=DIRECTION('',(0.,0.,1.));
#3348=DIRECTION('',(1.,0.,0.));
#3349=DIRECTION('',(0.,0.,1.));
#3350=DIRECTION('',(-1.,1.22464679914735E-16,0.));
#3351=DIRECTION('',(0.,0.,1.));
#3352=DIRECTION('',(1.,0.,0.));
#3353=DIRECTION('',(0.,0.,1.));
#3354=DIRECTION('',(1.,0.,0.));
#3355=DIRECTION('',(0.,0.,1.));
#3356=DIRECTION('',(1.,0.,0.));
#3357=DIRECTION('',(0.,0.,1.));
#3358=DIRECTION('',(1.,0.,0.));
#3359=DIRECTION('',(0.,0.,1.));
#3360=DIRECTION('',(1.,0.,0.));
#3361=DIRECTION('',(0.,0.,1.));
#3362=DIRECTION('',(1.,0.,0.));
#3363=DIRECTION('',(0.,0.,1.));
#3364=DIRECTION('',(1.,0.,0.));
#3365=DIRECTION('',(0.,0.,1.));
#3366=DIRECTION('',(1.,0.,0.));
#3367=DIRECTION('',(0.,0.,1.));
#3368=DIRECTION('',(1.,0.,0.));
#3369=DIRECTION('',(0.,0.,1.));
#3370=DIRECTION('',(-1.,1.22464679914735E-16,0.));
#3371=DIRECTION('',(0.,0.,1.));
#3372=DIRECTION('',(1.,0.,0.));
#3373=DIRECTION('',(0.,0.,1.));
#3374=DIRECTION('',(1.,0.,0.));
#3375=DIRECTION('',(0.,0.,1.));
#3376=DIRECTION('',(1.,0.,0.));
#3377=DIRECTION('',(0.,0.,1.));
#3378=DIRECTION('',(1.,0.,0.));
#3379=DIRECTION('',(0.,0.,1.));
#3380=DIRECTION('',(-1.,1.22464679914735E-16,0.));
#3381=DIRECTION('',(0.,0.,1.));
#3382=DIRECTION('',(-1.,1.22464679914735E-16,0.));
#3383=DIRECTION('',(0.,0.,1.));
#3384=DIRECTION('',(-1.,1.22464679914735E-16,0.));
#3385=DIRECTION('',(0.,0.,1.));
#3386=DIRECTION('',(-1.,1.22464679914735E-16,0.));
#3387=DIRECTION('',(0.,0.,1.));
#3388=DIRECTION('',(-1.,1.22464679914735E-16,0.));
#3389=DIRECTION('',(0.,0.,1.));
#3390=DIRECTION('',(-1.,1.22464679914735E-16,0.));
#3391=DIRECTION('',(0.,0.,1.));
#3392=DIRECTION('',(-1.,1.22464679914735E-16,0.));
#3393=DIRECTION('',(0.,0.,1.));
#3394=DIRECTION('',(-1.,1.22464679914735E-16,0.));
#3395=DIRECTION('',(0.,0.,1.));
#3396=DIRECTION('',(-1.,1.22464679914735E-16,0.));
#3397=DIRECTION('',(0.,0.,1.));
#3398=DIRECTION('',(1.,0.,0.));
#3399=DIRECTION('',(0.,0.,1.));
#3400=DIRECTION('',(-1.,1.22464679914735E-16,0.));
#3401=DIRECTION('',(0.,0.,1.));
#3402=DIRECTION('',(-1.,1.22464679914735E-16,0.));
#3403=DIRECTION('',(0.,0.,1.));
#3404=DIRECTION('',(-1.,1.22464679914735E-16,0.));
#3405=DIRECTION('',(0.,0.,1.));
#3406=DIRECTION('',(-1.,1.22464679914735E-16,0.));
#3407=DIRECTION('',(0.,0.,1.));
#3408=DIRECTION('',(1.,0.,0.));
#3409=DIRECTION('axis',(0.,0.,1.));
#3410=DIRECTION('refdir',(1.,0.,0.));
#3411=DIRECTION('axis',(0.,0.,1.));
#3412=DIRECTION('refdir',(1.,0.,0.));
#3413=DIRECTION('center_axis',(0.,1.,0.));
#3414=DIRECTION('ref_axis',(1.,0.,0.));
#3415=DIRECTION('center_axis',(0.,1.,0.));
#3416=DIRECTION('ref_axis',(1.,0.,0.));
#3417=DIRECTION('',(0.,1.,0.));
#3418=DIRECTION('center_axis',(0.,-1.,0.));
#3419=DIRECTION('ref_axis',(1.,0.,0.));
#3420=DIRECTION('center_axis',(0.,1.,0.));
#3421=DIRECTION('ref_axis',(1.,0.,0.));
#3422=DIRECTION('center_axis',(0.,1.,0.));
#3423=DIRECTION('ref_axis',(1.,0.,0.));
#3424=DIRECTION('center_axis',(0.,1.,0.));
#3425=DIRECTION('ref_axis',(1.,0.,0.));
#3426=DIRECTION('center_axis',(0.,1.,0.));
#3427=DIRECTION('ref_axis',(1.,0.,0.));
#3428=DIRECTION('',(0.,1.,0.));
#3429=DIRECTION('center_axis',(0.,1.,0.));
#3430=DIRECTION('ref_axis',(1.,0.,0.));
#3431=DIRECTION('center_axis',(0.,1.,0.));
#3432=DIRECTION('ref_axis',(1.,0.,0.));
#3433=DIRECTION('center_axis',(0.,-1.,0.));
#3434=DIRECTION('ref_axis',(1.,0.,0.));
#3435=DIRECTION('center_axis',(0.,1.,0.));
#3436=DIRECTION('ref_axis',(1.,0.,0.));
#3437=DIRECTION('',(0.,1.,0.));
#3438=DIRECTION('center_axis',(0.,1.,0.));
#3439=DIRECTION('ref_axis',(1.,0.,0.));
#3440=DIRECTION('center_axis',(0.,1.,0.));
#3441=DIRECTION('ref_axis',(1.,0.,0.));
#3442=DIRECTION('',(0.,-1.,0.));
#3443=DIRECTION('center_axis',(0.,1.,0.));
#3444=DIRECTION('ref_axis',(1.,0.,0.));
#3445=DIRECTION('center_axis',(0.,1.,0.));
#3446=DIRECTION('ref_axis',(1.,0.,0.));
#3447=DIRECTION('center_axis',(0.,1.,0.));
#3448=DIRECTION('ref_axis',(1.,0.,0.));
#3449=DIRECTION('axis',(0.,0.,1.));
#3450=DIRECTION('refdir',(1.,0.,0.));
#3451=DIRECTION('axis',(0.,0.,1.));
#3452=DIRECTION('refdir',(1.,0.,0.));
#3453=DIRECTION('center_axis',(0.,-1.,0.));
#3454=DIRECTION('ref_axis',(0.,0.,-1.));
#3455=DIRECTION('center_axis',(0.,-1.,0.));
#3456=DIRECTION('ref_axis',(1.,0.,0.));
#3457=DIRECTION('center_axis',(0.,-1.,0.));
#3458=DIRECTION('ref_axis',(1.,0.,0.));
#3459=DIRECTION('center_axis',(1.,0.,1.22464679914735E-16));
#3460=DIRECTION('ref_axis',(-1.22464679914735E-16,0.,1.));
#3461=DIRECTION('center_axis',(0.,1.,0.));
#3462=DIRECTION('ref_axis',(1.,0.,0.));
#3463=DIRECTION('center_axis',(0.,1.,0.));
#3464=DIRECTION('ref_axis',(1.,0.,0.));
#3465=DIRECTION('center_axis',(0.,-1.,0.));
#3466=DIRECTION('ref_axis',(1.,0.,0.));
#3467=DIRECTION('',(0.,1.,0.));
#3468=DIRECTION('center_axis',(0.,-1.,0.));
#3469=DIRECTION('ref_axis',(1.,0.,0.));
#3470=DIRECTION('center_axis',(0.,-1.,0.));
#3471=DIRECTION('ref_axis',(1.,0.,0.));
#3472=DIRECTION('center_axis',(0.,-1.,0.));
#3473=DIRECTION('ref_axis',(1.,0.,0.));
#3474=DIRECTION('',(0.,1.,0.));
#3475=DIRECTION('center_axis',(0.,-1.,0.));
#3476=DIRECTION('ref_axis',(1.,0.,0.));
#3477=DIRECTION('center_axis',(0.,1.,0.));
#3478=DIRECTION('ref_axis',(1.,0.,0.));
#3479=DIRECTION('',(-0.707106781186548,0.707106781186547,-8.65956056235493E-17));
#3480=DIRECTION('center_axis',(0.,-1.,0.));
#3481=DIRECTION('ref_axis',(1.,0.,0.));
#3482=DIRECTION('center_axis',(0.,1.,0.));
#3483=DIRECTION('ref_axis',(0.,0.,1.));
#3484=DIRECTION('center_axis',(0.,-1.,0.));
#3485=DIRECTION('ref_axis',(1.,0.,0.));
#3486=DIRECTION('center_axis',(0.,-1.,0.));
#3487=DIRECTION('ref_axis',(1.,0.,0.));
#3488=DIRECTION('',(0.,1.,0.));
#3489=DIRECTION('center_axis',(0.,-1.,0.));
#3490=DIRECTION('ref_axis',(0.,0.,-1.));
#3491=DIRECTION('center_axis',(0.,-1.,0.));
#3492=DIRECTION('ref_axis',(1.,0.,0.));
#3493=DIRECTION('center_axis',(0.,-1.,0.));
#3494=DIRECTION('ref_axis',(1.,0.,0.));
#3495=DIRECTION('',(0.707106781186548,0.707106781186547,8.65956056235493E-17));
#3496=DIRECTION('axis',(0.,0.,1.));
#3497=DIRECTION('refdir',(1.,0.,0.));
#3498=DIRECTION('center_axis',(0.,-1.,0.));
#3499=DIRECTION('ref_axis',(0.,0.,-1.));
#3500=DIRECTION('center_axis',(0.,-1.,0.));
#3501=DIRECTION('ref_axis',(1.,0.,0.));
#3502=DIRECTION('center_axis',(0.,-1.,0.));
#3503=DIRECTION('ref_axis',(1.,0.,0.));
#3504=DIRECTION('center_axis',(1.,0.,1.22464679914735E-16));
#3505=DIRECTION('ref_axis',(-1.22464679914735E-16,0.,1.));
#3506=DIRECTION('center_axis',(0.,1.,0.));
#3507=DIRECTION('ref_axis',(1.,0.,0.));
#3508=DIRECTION('center_axis',(0.,1.,0.));
#3509=DIRECTION('ref_axis',(1.,0.,0.));
#3510=DIRECTION('center_axis',(0.,-1.,0.));
#3511=DIRECTION('ref_axis',(1.,0.,0.));
#3512=DIRECTION('center_axis',(0.,-1.,0.));
#3513=DIRECTION('ref_axis',(1.,0.,0.));
#3514=DIRECTION('',(0.,1.,0.));
#3515=DIRECTION('center_axis',(0.,1.,0.));
#3516=DIRECTION('ref_axis',(0.,0.,1.));
#3517=DIRECTION('center_axis',(0.,-1.,0.));
#3518=DIRECTION('ref_axis',(1.,0.,0.));
#3519=DIRECTION('center_axis',(0.,-1.,0.));
#3520=DIRECTION('ref_axis',(1.,0.,0.));
#3521=DIRECTION('center_axis',(0.,-1.,0.));
#3522=DIRECTION('ref_axis',(1.,0.,0.));
#3523=DIRECTION('center_axis',(0.,-1.,0.));
#3524=DIRECTION('ref_axis',(1.,0.,0.));
#3525=DIRECTION('',(0.707106781186548,0.707106781186547,8.65956056235494E-17));
#3526=DIRECTION('center_axis',(0.,-1.,0.));
#3527=DIRECTION('ref_axis',(1.,0.,0.));
#3528=DIRECTION('center_axis',(0.,-1.,0.));
#3529=DIRECTION('ref_axis',(1.,0.,0.));
#3530=DIRECTION('',(0.,1.,0.));
#3531=DIRECTION('center_axis',(0.,1.,0.));
#3532=DIRECTION('ref_axis',(1.,0.,0.));
#3533=DIRECTION('center_axis',(0.,-1.,0.));
#3534=DIRECTION('ref_axis',(1.,0.,0.));
#3535=DIRECTION('',(-0.707106781186548,0.707106781186547,-8.65956056235494E-17));
#3536=DIRECTION('center_axis',(0.,-1.,0.));
#3537=DIRECTION('ref_axis',(0.,0.,-1.));
#3538=DIRECTION('center_axis',(0.,-1.,0.));
#3539=DIRECTION('ref_axis',(1.,0.,0.));
#3540=DIRECTION('',(0.,1.,0.));
#3541=DIRECTION('axis',(0.,0.,1.));
#3542=DIRECTION('refdir',(1.,0.,0.));
#3543=DIRECTION('center_axis',(0.,0.,1.));
#3544=DIRECTION('ref_axis',(1.,0.,0.));
#3545=DIRECTION('center_axis',(1.22464679914735E-16,-1.,0.));
#3546=DIRECTION('ref_axis',(-1.,-1.22464679914735E-16,0.));
#3547=DIRECTION('center_axis',(0.78183148246803,0.,0.623489801858733));
#3548=DIRECTION('ref_axis',(0.623489801858734,0.,-0.78183148246803));
#3549=DIRECTION('center_axis',(7.63554790147315E-17,-1.,-9.57467422477103E-17));
#3550=DIRECTION('ref_axis',(-0.623489801858734,-1.22464679914735E-16,0.78183148246803));
#3551=DIRECTION('center_axis',(0.974927912181824,0.,-0.222520933956314));
#3552=DIRECTION('ref_axis',(-0.222520933956314,0.,-0.974927912181824));
#3553=DIRECTION('center_axis',(-2.7250954951288E-17,-1.,-1.19394234705288E-16));
#3554=DIRECTION('ref_axis',(0.222520933956314,-1.22464679914735E-16,0.974927912181824));
#3555=DIRECTION('center_axis',(0.433883739117558,0.,-0.900968867902419));
#3556=DIRECTION('ref_axis',(-0.900968867902419,0.,-0.433883739117558));
#3557=DIRECTION('center_axis',(-1.10336864020811E-16,-1.,-5.31354332312403E-17));
#3558=DIRECTION('ref_axis',(0.900968867902419,-1.22464679914735E-16,0.433883739117558));
#3559=DIRECTION('center_axis',(-0.433883739117558,0.,-0.900968867902419));
#3560=DIRECTION('ref_axis',(-0.900968867902419,0.,0.433883739117558));
#3561=DIRECTION('center_axis',(-1.10336864020811E-16,-1.,5.31354332312403E-17));
#3562=DIRECTION('ref_axis',(0.900968867902419,-1.22464679914735E-16,-0.433883739117558));
#3563=DIRECTION('center_axis',(-0.974927912181824,0.,-0.222520933956314));
#3564=DIRECTION('ref_axis',(-0.222520933956315,0.,0.974927912181824));
#3565=DIRECTION('center_axis',(-2.7250954951288E-17,-1.,1.19394234705288E-16));
#3566=DIRECTION('ref_axis',(0.222520933956315,-1.22464679914735E-16,-0.974927912181824));
#3567=DIRECTION('center_axis',(-0.78183148246803,0.,0.623489801858734));
#3568=DIRECTION('ref_axis',(0.623489801858733,0.,0.78183148246803));
#3569=DIRECTION('center_axis',(7.63554790147315E-17,-1.,9.57467422477103E-17));
#3570=DIRECTION('ref_axis',(-0.623489801858733,-1.22464679914735E-16,-0.78183148246803));
#3571=DIRECTION('axis',(0.,0.,1.));
#3572=DIRECTION('refdir',(1.,0.,0.));
#3573=DIRECTION('center_axis',(0.,0.,1.));
#3574=DIRECTION('ref_axis',(1.,0.,0.));
#3575=DIRECTION('center_axis',(0.,-1.,0.));
#3576=DIRECTION('ref_axis',(0.,0.,-1.));
#3577=DIRECTION('center_axis',(0.,-1.,0.));
#3578=DIRECTION('ref_axis',(0.,0.,-1.));
#3579=DIRECTION('center_axis',(0.,1.,0.));
#3580=DIRECTION('ref_axis',(1.,0.,0.));
#3581=DIRECTION('center_axis',(0.,1.,0.));
#3582=DIRECTION('ref_axis',(1.,0.,0.));
#3583=DIRECTION('center_axis',(0.,1.,0.));
#3584=DIRECTION('ref_axis',(1.,0.,0.));
#3585=DIRECTION('center_axis',(0.,1.,0.));
#3586=DIRECTION('ref_axis',(1.,0.,0.));
#3587=DIRECTION('',(0.,-1.,0.));
#3588=DIRECTION('center_axis',(0.,-1.,0.));
#3589=DIRECTION('ref_axis',(1.,0.,0.));
#3590=DIRECTION('center_axis',(0.,1.,0.));
#3591=DIRECTION('ref_axis',(1.,0.,0.));
#3592=DIRECTION('center_axis',(0.,1.,0.));
#3593=DIRECTION('ref_axis',(1.,0.,0.));
#3594=DIRECTION('center_axis',(0.,1.,0.));
#3595=DIRECTION('ref_axis',(1.,0.,0.));
#3596=DIRECTION('center_axis',(0.,1.,0.));
#3597=DIRECTION('ref_axis',(1.,0.,0.));
#3598=DIRECTION('center_axis',(0.,1.,0.));
#3599=DIRECTION('ref_axis',(1.,0.,0.));
#3600=DIRECTION('center_axis',(0.,1.,0.));
#3601=DIRECTION('ref_axis',(1.,0.,0.));
#3602=DIRECTION('center_axis',(0.,-1.,0.));
#3603=DIRECTION('ref_axis',(1.,0.,0.));
#3604=DIRECTION('center_axis',(0.,-1.,0.));
#3605=DIRECTION('ref_axis',(0.,0.,-1.));
#3606=DIRECTION('center_axis',(8.96625347776458E-17,0.,1.));
#3607=DIRECTION('ref_axis',(1.,0.,0.));
#3608=DIRECTION('center_axis',(0.,-1.,0.));
#3609=DIRECTION('ref_axis',(0.,0.,-1.));
#3610=DIRECTION('center_axis',(0.,1.,0.));
#3611=DIRECTION('ref_axis',(1.,0.,0.));
#3612=DIRECTION('center_axis',(0.,-1.,0.));
#3613=DIRECTION('ref_axis',(1.,0.,0.));
#3614=DIRECTION('center_axis',(0.,-1.,0.));
#3615=DIRECTION('ref_axis',(0.,0.,-1.));
#3616=DIRECTION('center_axis',(0.,0.,1.));
#3617=DIRECTION('ref_axis',(1.,0.,0.));
#3618=DIRECTION('center_axis',(0.,-1.,0.));
#3619=DIRECTION('ref_axis',(0.,0.,-1.));
#3620=DIRECTION('center_axis',(0.,1.,0.));
#3621=DIRECTION('ref_axis',(1.,0.,0.));
#3622=DIRECTION('center_axis',(0.,-1.,0.));
#3623=DIRECTION('ref_axis',(1.,0.,0.));
#3624=DIRECTION('center_axis',(0.,-1.,0.));
#3625=DIRECTION('ref_axis',(1.,0.,0.));
#3626=DIRECTION('center_axis',(0.,-1.,0.));
#3627=DIRECTION('ref_axis',(0.,0.,-1.));
#3628=DIRECTION('center_axis',(0.,0.,1.));
#3629=DIRECTION('ref_axis',(1.,0.,0.));
#3630=DIRECTION('center_axis',(0.,-1.,0.));
#3631=DIRECTION('ref_axis',(0.,0.,-1.));
#3632=DIRECTION('center_axis',(0.,1.,0.));
#3633=DIRECTION('ref_axis',(1.,0.,0.));
#3634=DIRECTION('center_axis',(0.,-1.,0.));
#3635=DIRECTION('ref_axis',(1.,0.,0.));
#3636=DIRECTION('center_axis',(0.,-1.,0.));
#3637=DIRECTION('ref_axis',(0.,0.,-1.));
#3638=DIRECTION('center_axis',(8.96625347776458E-17,0.,1.));
#3639=DIRECTION('ref_axis',(1.,0.,0.));
#3640=DIRECTION('center_axis',(0.,-1.,0.));
#3641=DIRECTION('ref_axis',(0.,0.,-1.));
#3642=DIRECTION('center_axis',(0.,1.,0.));
#3643=DIRECTION('ref_axis',(1.,0.,0.));
#3644=DIRECTION('center_axis',(0.,-1.,0.));
#3645=DIRECTION('ref_axis',(1.,0.,0.));
#3646=DIRECTION('center_axis',(0.,-1.,0.));
#3647=DIRECTION('ref_axis',(0.,0.,-1.));
#3648=DIRECTION('center_axis',(0.,0.,1.));
#3649=DIRECTION('ref_axis',(1.,0.,0.));
#3650=DIRECTION('center_axis',(0.,-1.,0.));
#3651=DIRECTION('ref_axis',(0.,0.,-1.));
#3652=DIRECTION('center_axis',(0.,1.,0.));
#3653=DIRECTION('ref_axis',(1.,0.,0.));
#3654=DIRECTION('center_axis',(0.,1.,0.));
#3655=DIRECTION('ref_axis',(1.,0.,0.));
#3656=DIRECTION('',(0.,1.,0.));
#3657=DIRECTION('center_axis',(0.,-1.,0.));
#3658=DIRECTION('ref_axis',(1.,0.,0.));
#3659=DIRECTION('center_axis',(0.,-1.,0.));
#3660=DIRECTION('ref_axis',(1.,0.,0.));
#3661=DIRECTION('center_axis',(0.,1.,0.));
#3662=DIRECTION('ref_axis',(1.,0.,0.));
#3663=DIRECTION('center_axis',(0.,-1.,0.));
#3664=DIRECTION('ref_axis',(0.,0.,-1.));
#3665=DIRECTION('center_axis',(0.,0.,1.));
#3666=DIRECTION('ref_axis',(1.,0.,0.));
#3667=DIRECTION('center_axis',(0.,-1.,0.));
#3668=DIRECTION('ref_axis',(0.,0.,-1.));
#3669=DIRECTION('center_axis',(0.,-1.,0.));
#3670=DIRECTION('ref_axis',(-1.,0.,0.));
#3671=DIRECTION('center_axis',(0.,1.,0.));
#3672=DIRECTION('ref_axis',(1.,0.,0.));
#3673=DIRECTION('axis',(0.,0.,1.));
#3674=DIRECTION('refdir',(1.,0.,0.));
#3675=DIRECTION('center_axis',(0.,1.,0.));
#3676=DIRECTION('ref_axis',(0.,0.,1.));
#3677=DIRECTION('center_axis',(0.,-1.,0.));
#3678=DIRECTION('ref_axis',(1.,0.,0.));
#3679=DIRECTION('center_axis',(0.,-1.,0.));
#3680=DIRECTION('ref_axis',(1.,0.,0.));
#3681=DIRECTION('center_axis',(0.,-1.,0.));
#3682=DIRECTION('ref_axis',(1.,0.,0.));
#3683=DIRECTION('center_axis',(0.,-1.,0.));
#3684=DIRECTION('ref_axis',(1.,0.,0.));
#3685=DIRECTION('',(0.,1.,0.));
#3686=DIRECTION('center_axis',(0.,-1.,0.));
#3687=DIRECTION('ref_axis',(0.,0.,-1.));
#3688=DIRECTION('center_axis',(0.,-1.,0.));
#3689=DIRECTION('ref_axis',(1.,0.,0.));
#3690=DIRECTION('center_axis',(0.,-1.,0.));
#3691=DIRECTION('ref_axis',(1.,0.,0.));
#3692=DIRECTION('',(0.,1.,0.));
#3693=DIRECTION('center_axis',(0.,1.,0.));
#3694=DIRECTION('ref_axis',(0.,0.,1.));
#3695=DIRECTION('center_axis',(0.,-1.,0.));
#3696=DIRECTION('ref_axis',(1.,0.,0.));
#3697=DIRECTION('center_axis',(0.,-1.,0.));
#3698=DIRECTION('ref_axis',(1.,0.,0.));
#3699=DIRECTION('center_axis',(0.,-1.,0.));
#3700=DIRECTION('ref_axis',(1.,0.,0.));
#3701=DIRECTION('center_axis',(0.,-1.,0.));
#3702=DIRECTION('ref_axis',(1.,0.,0.));
#3703=DIRECTION('',(0.,1.,0.));
#3704=DIRECTION('center_axis',(0.,-1.,0.));
#3705=DIRECTION('ref_axis',(0.,0.,-1.));
#3706=DIRECTION('center_axis',(0.,-1.,0.));
#3707=DIRECTION('ref_axis',(1.,0.,0.));
#3708=DIRECTION('center_axis',(0.,-1.,0.));
#3709=DIRECTION('ref_axis',(1.,0.,0.));
#3710=DIRECTION('',(0.,1.,0.));
#3711=DIRECTION('',(0.,0.,1.));
#3712=DIRECTION('',(1.,0.,0.));
#3713=DIRECTION('',(0.,0.,1.));
#3714=DIRECTION('',(1.,0.,0.));
#3715=DIRECTION('',(0.,0.,1.));
#3716=DIRECTION('',(1.,0.,0.));
#3717=DIRECTION('',(0.,0.,1.));
#3718=DIRECTION('',(1.,0.,0.));
#3719=DIRECTION('',(0.,0.,1.));
#3720=DIRECTION('',(1.,0.,0.));
#3721=DIRECTION('axis',(0.,0.,1.));
#3722=DIRECTION('refdir',(1.,0.,0.));
#3723=DIRECTION('center_axis',(0.,1.,0.));
#3724=DIRECTION('ref_axis',(1.,0.,0.));
#3725=DIRECTION('center_axis',(0.,-1.,0.));
#3726=DIRECTION('ref_axis',(1.,0.,0.));
#3727=DIRECTION('',(0.,-1.,0.));
#3728=DIRECTION('center_axis',(0.,-1.,0.));
#3729=DIRECTION('ref_axis',(1.,0.,0.));
#3730=DIRECTION('center_axis',(0.,1.,0.));
#3731=DIRECTION('ref_axis',(1.,0.,0.));
#3732=DIRECTION('center_axis',(0.,1.,0.));
#3733=DIRECTION('ref_axis',(1.,0.,0.));
#3734=DIRECTION('',(0.,-1.,0.));
#3735=DIRECTION('center_axis',(0.,1.,0.));
#3736=DIRECTION('ref_axis',(1.,0.,0.));
#3737=DIRECTION('center_axis',(0.,1.,0.));
#3738=DIRECTION('ref_axis',(1.,0.,0.));
#3739=DIRECTION('center_axis',(0.,1.,0.));
#3740=DIRECTION('ref_axis',(1.,0.,0.));
#3741=DIRECTION('',(0.,0.,1.));
#3742=DIRECTION('',(1.,0.,0.));
#3743=DIRECTION('',(0.,0.,1.));
#3744=DIRECTION('',(1.,0.,0.));
#3745=DIRECTION('',(0.,0.,1.));
#3746=DIRECTION('',(1.,0.,0.));
#3747=DIRECTION('',(0.,0.,1.));
#3748=DIRECTION('',(1.,0.,0.));
#3749=DIRECTION('',(0.,0.,1.));
#3750=DIRECTION('',(1.,0.,0.));
#3751=DIRECTION('',(0.,0.,1.));
#3752=DIRECTION('',(1.,0.,0.));
#3753=DIRECTION('',(0.,0.,1.));
#3754=DIRECTION('',(1.,0.,0.));
#3755=DIRECTION('',(-0.0576975931199009,1.0698906979028E-15,0.998334106273131));
#3756=DIRECTION('',(0.998334106273132,-7.51433311950164E-16,0.0576975931199052));
#3757=DIRECTION('',(-0.0461840073097409,6.55136953588178E-18,0.998932949435954));
#3758=DIRECTION('',(0.998932949435955,1.66006395712964E-16,0.046184007309741));
#3759=DIRECTION('',(0.0235818179453089,-6.16973863065135E-16,0.999721910264246));
#3760=DIRECTION('',(0.999721910264248,-1.45112820548935E-17,-0.0235818179453101));
#3761=CARTESIAN_POINT('',(0.,0.,0.));
#3762=CARTESIAN_POINT('',(0.,0.,0.));
#3763=CARTESIAN_POINT('',(0.,0.,0.));
#3764=CARTESIAN_POINT('Origin',(-1.5,3.5,7.5));
#3765=CARTESIAN_POINT('',(-1.84,3.5,7.5));
#3766=CARTESIAN_POINT('Origin',(-1.5,3.5,7.5));
#3767=CARTESIAN_POINT('',(-1.84,5.5,7.5));
#3768=CARTESIAN_POINT('',(-1.84,3.5,7.5));
#3769=CARTESIAN_POINT('Origin',(-1.5,5.5,7.5));
#3770=CARTESIAN_POINT('Origin',(-1.5,3.5,7.5));
#3771=CARTESIAN_POINT('Origin',(1.5,3.5,7.5));
#3772=CARTESIAN_POINT('',(1.16,3.5,7.5));
#3773=CARTESIAN_POINT('Origin',(1.5,3.5,7.5));
#3774=CARTESIAN_POINT('',(1.16,5.5,7.5));
#3775=CARTESIAN_POINT('',(1.16,3.5,7.5));
#3776=CARTESIAN_POINT('Origin',(1.5,5.5,7.5));
#3777=CARTESIAN_POINT('Origin',(1.5,3.5,7.5));
#3778=CARTESIAN_POINT('Origin',(-1.5,-5.6,7.5));
#3779=CARTESIAN_POINT('',(-1.84,-5.5,7.5));
#3780=CARTESIAN_POINT('Origin',(-1.5,-5.5,7.5));
#3781=CARTESIAN_POINT('',(-1.84,-3.5,7.5));
#3782=CARTESIAN_POINT('',(-1.84,-5.6,7.5));
#3783=CARTESIAN_POINT('Origin',(-1.5,-3.5,7.5));
#3784=CARTESIAN_POINT('Origin',(-1.5,-3.5,7.5));
#3785=CARTESIAN_POINT('Origin',(1.5,-5.6,7.5));
#3786=CARTESIAN_POINT('',(1.16,-5.5,7.5));
#3787=CARTESIAN_POINT('Origin',(1.5,-5.5,7.5));
#3788=CARTESIAN_POINT('',(1.16,-3.5,7.5));
#3789=CARTESIAN_POINT('',(1.16,-5.6,7.5));
#3790=CARTESIAN_POINT('Origin',(1.5,-3.5,7.5));
#3791=CARTESIAN_POINT('Origin',(1.5,-3.5,7.5));
#3792=CARTESIAN_POINT('Origin',(2.5,5.5,7.));
#3793=CARTESIAN_POINT('',(2.5,5.5,7.));
#3794=CARTESIAN_POINT('',(-2.5,5.5,7.));
#3795=CARTESIAN_POINT('',(2.5,5.5,7.));
#3796=CARTESIAN_POINT('',(-2.5,5.5,8.));
#3797=CARTESIAN_POINT('',(-2.5,5.5,7.));
#3798=CARTESIAN_POINT('',(2.5,5.5,8.));
#3799=CARTESIAN_POINT('',(2.5,5.5,8.));
#3800=CARTESIAN_POINT('',(2.5,5.5,7.));
#3801=CARTESIAN_POINT('Origin',(2.5,-5.5,7.));
#3802=CARTESIAN_POINT('',(2.5,-5.5,7.));
#3803=CARTESIAN_POINT('',(2.5,-5.5,7.));
#3804=CARTESIAN_POINT('',(2.5,-5.5,8.));
#3805=CARTESIAN_POINT('',(2.5,-5.5,8.));
#3806=CARTESIAN_POINT('',(2.5,-5.5,7.));
#3807=CARTESIAN_POINT('Origin',(-2.5,-5.5,7.));
#3808=CARTESIAN_POINT('',(-2.5,-5.5,7.));
#3809=CARTESIAN_POINT('',(-2.5,-5.5,7.));
#3810=CARTESIAN_POINT('',(-2.5,-5.5,8.));
#3811=CARTESIAN_POINT('',(-2.5,-5.5,8.));
#3812=CARTESIAN_POINT('',(-2.5,-5.5,7.));
#3813=CARTESIAN_POINT('Origin',(-2.5,5.5,7.));
#3814=CARTESIAN_POINT('',(-2.5,5.5,7.));
#3815=CARTESIAN_POINT('',(-2.5,5.5,8.));
#3816=CARTESIAN_POINT('Origin',(0.,0.,8.));
#3817=CARTESIAN_POINT('Origin',(0.,0.,7.));
#3818=CARTESIAN_POINT('',(0.,0.,0.));
#3819=CARTESIAN_POINT('Origin',(-1.5,5.4,7.5));
#3820=CARTESIAN_POINT('',(-1.925,5.5,7.5));
#3821=CARTESIAN_POINT('Origin',(-1.5,5.5,7.5));
#3822=CARTESIAN_POINT('',(-1.925,6.3,7.5));
#3823=CARTESIAN_POINT('',(-1.925,5.4,7.5));
#3824=CARTESIAN_POINT('Origin',(-1.5,6.3,7.5));
#3825=CARTESIAN_POINT('Origin',(1.5,5.4,7.5));
#3826=CARTESIAN_POINT('',(1.075,5.5,7.5));
#3827=CARTESIAN_POINT('Origin',(1.5,5.5,7.5));
#3828=CARTESIAN_POINT('',(1.075,6.3,7.5));
#3829=CARTESIAN_POINT('',(1.075,5.4,7.5));
#3830=CARTESIAN_POINT('Origin',(1.5,6.3,7.5));
#3831=CARTESIAN_POINT('Origin',(-5.,5.4,13.75));
#3832=CARTESIAN_POINT('',(-5.6,5.5,13.75));
#3833=CARTESIAN_POINT('Origin',(-5.,5.5,13.75));
#3834=CARTESIAN_POINT('',(-5.6,6.3,13.75));
#3835=CARTESIAN_POINT('',(-5.6,5.4,13.75));
#3836=CARTESIAN_POINT('Origin',(-5.,6.3,13.75));
#3837=CARTESIAN_POINT('Origin',(5.,5.4,13.75));
#3838=CARTESIAN_POINT('',(4.4,5.5,13.75));
#3839=CARTESIAN_POINT('Origin',(5.,5.5,13.75));
#3840=CARTESIAN_POINT('',(4.4,6.3,13.75));
#3841=CARTESIAN_POINT('',(4.4,5.4,13.75));
#3842=CARTESIAN_POINT('Origin',(5.,6.3,13.75));
#3843=CARTESIAN_POINT('Origin',(8.,6.3,7.));
#3844=CARTESIAN_POINT('',(8.,6.3,7.));
#3845=CARTESIAN_POINT('',(-8.,6.3,7.));
#3846=CARTESIAN_POINT('',(8.,6.3,7.));
#3847=CARTESIAN_POINT('',(-8.,6.3,16.));
#3848=CARTESIAN_POINT('',(-8.,6.3,7.));
#3849=CARTESIAN_POINT('',(8.,6.3,16.));
#3850=CARTESIAN_POINT('',(8.,6.3,16.));
#3851=CARTESIAN_POINT('',(8.,6.3,7.));
#3852=CARTESIAN_POINT('Origin',(8.,5.5,7.));
#3853=CARTESIAN_POINT('',(8.,5.5,7.));
#3854=CARTESIAN_POINT('',(8.,5.5,7.));
#3855=CARTESIAN_POINT('',(8.,5.5,16.));
#3856=CARTESIAN_POINT('',(8.,5.5,16.));
#3857=CARTESIAN_POINT('',(8.,5.5,7.));
#3858=CARTESIAN_POINT('Origin',(-8.,5.5,7.));
#3859=CARTESIAN_POINT('',(-8.,5.5,7.));
#3860=CARTESIAN_POINT('',(-8.,5.5,7.));
#3861=CARTESIAN_POINT('',(-8.,5.5,16.));
#3862=CARTESIAN_POINT('',(-8.,5.5,16.));
#3863=CARTESIAN_POINT('',(-8.,5.5,7.));
#3864=CARTESIAN_POINT('Origin',(-8.,6.3,7.));
#3865=CARTESIAN_POINT('',(-8.,6.3,7.));
#3866=CARTESIAN_POINT('',(-8.,6.3,16.));
#3867=CARTESIAN_POINT('Origin',(0.,5.9,16.));
#3868=CARTESIAN_POINT('Origin',(0.,5.9,7.));
#3869=CARTESIAN_POINT('',(0.,0.,0.));
#3870=CARTESIAN_POINT('Origin',(-21.,-0.7,-2.));
#3871=CARTESIAN_POINT('',(-21.51,-0.6,-2.));
#3872=CARTESIAN_POINT('Origin',(-21.,-0.6,-2.));
#3873=CARTESIAN_POINT('',(-21.51,0.6,-2.));
#3874=CARTESIAN_POINT('',(-21.51,-0.7,-2.));
#3875=CARTESIAN_POINT('Origin',(-21.,0.6,-2.));
#3876=CARTESIAN_POINT('Origin',(-23.,-0.6,-2.));
#3877=CARTESIAN_POINT('',(-23.,-0.6,0.));
#3878=CARTESIAN_POINT('',(-23.,-0.6,-2.));
#3879=CARTESIAN_POINT('',(-23.,-0.6,0.));
#3880=CARTESIAN_POINT('',(-23.,0.6,0.));
#3881=CARTESIAN_POINT('',(-23.,-0.6,0.));
#3882=CARTESIAN_POINT('',(-23.,0.6,-2.));
#3883=CARTESIAN_POINT('',(-23.,0.6,0.));
#3884=CARTESIAN_POINT('',(-23.,-0.6,-2.));
#3885=CARTESIAN_POINT('Origin',(-19.,-0.6,0.));
#3886=CARTESIAN_POINT('',(-19.,-0.6,-2.));
#3887=CARTESIAN_POINT('',(-19.,-0.6,0.));
#3888=CARTESIAN_POINT('',(-19.,-0.6,-2.));
#3889=CARTESIAN_POINT('',(-19.,0.6,-2.));
#3890=CARTESIAN_POINT('',(-19.,-0.6,-2.));
#3891=CARTESIAN_POINT('',(-19.,0.6,0.));
#3892=CARTESIAN_POINT('',(-19.,0.6,-2.));
#3893=CARTESIAN_POINT('',(-19.,-0.6,0.));
#3894=CARTESIAN_POINT('Origin',(-23.,-0.6,0.));
#3895=CARTESIAN_POINT('',(-19.,0.6,0.));
#3896=CARTESIAN_POINT('',(-19.,-0.6,0.));
#3897=CARTESIAN_POINT('Origin',(-21.,0.6,-2.));
#3898=CARTESIAN_POINT('Origin',(-21.,0.6,-2.));
#3899=CARTESIAN_POINT('Origin',(-21.,-0.6,-2.));
#3900=CARTESIAN_POINT('Origin',(-21.,-0.6,-2.));
#3901=CARTESIAN_POINT('Origin',(-21.,-0.6,-2.));
#3902=CARTESIAN_POINT('',(0.,0.,0.));
#3903=CARTESIAN_POINT('Origin',(0.,0.,0.));
#3904=CARTESIAN_POINT('',(-0.42,0.16,5.14351655641888E-17));
#3905=CARTESIAN_POINT('Origin',(0.,0.16,0.));
#3906=CARTESIAN_POINT('',(-0.42,0.,5.14351655641888E-17));
#3907=CARTESIAN_POINT('',(-0.42,0.,5.14351655641888E-17));
#3908=CARTESIAN_POINT('Origin',(0.,0.,0.));
#3909=CARTESIAN_POINT('Origin',(0.,0.,0.));
#3910=CARTESIAN_POINT('',(-0.8,0.16,9.79717439317883E-17));
#3911=CARTESIAN_POINT('Origin',(0.,0.16,0.));
#3912=CARTESIAN_POINT('',(-0.8,0.,9.79717439317883E-17));
#3913=CARTESIAN_POINT('',(-0.8,0.,9.79717439317883E-17));
#3914=CARTESIAN_POINT('Origin',(0.,0.,0.));
#3915=CARTESIAN_POINT('Origin',(0.,0.16,0.));
#3916=CARTESIAN_POINT('Origin',(0.,0.,0.));
#3917=CARTESIAN_POINT('',(0.,0.,0.));
#3918=CARTESIAN_POINT('Origin',(0.6,0.8,0.));
#3919=CARTESIAN_POINT('',(-0.6,0.8,-7.34788079488412E-17));
#3920=CARTESIAN_POINT('Origin',(0.,0.8,0.));
#3921=CARTESIAN_POINT('Origin',(0.,0.775,0.));
#3922=CARTESIAN_POINT('',(-0.65,0.75,-7.9602041944578E-17));
#3923=CARTESIAN_POINT('Origin',(0.,0.75,0.));
#3924=CARTESIAN_POINT('',(-0.625,0.775,-7.65404249467096E-17));
#3925=CARTESIAN_POINT('Origin',(0.,0.39,0.));
#3926=CARTESIAN_POINT('',(-0.65,0.0299999999999998,-7.9602041944578E-17));
#3927=CARTESIAN_POINT('Origin',(0.,0.0299999999999998,0.));
#3928=CARTESIAN_POINT('',(-0.65,0.39,-7.9602041944578E-17));
#3929=CARTESIAN_POINT('Origin',(0.,0.0150000000000001,0.));
#3930=CARTESIAN_POINT('',(-0.62,5.89805981832114E-17,-7.59281015471359E-17));
#3931=CARTESIAN_POINT('Origin',(0.,0.,0.));
#3932=CARTESIAN_POINT('',(-0.635,0.0150000000000001,-7.77650717458569E-17));
#3933=CARTESIAN_POINT('Origin',(0.42,0.,0.));
#3934=CARTESIAN_POINT('',(-0.42,-3.46944695195361E-18,-5.14351655641888E-17));
#3935=CARTESIAN_POINT('Origin',(0.,0.,0.));
#3936=CARTESIAN_POINT('Origin',(0.,-0.02,0.));
#3937=CARTESIAN_POINT('',(-0.3933,-0.0534000000000001,4.81653586104654E-17));
#3938=CARTESIAN_POINT('Origin',(0.,-0.0534000000000001,0.));
#3939=CARTESIAN_POINT('',(-0.41,-0.02,-5.02105187650415E-17));
#3940=CARTESIAN_POINT('Origin',(0.,-1.48,0.));
#3941=CARTESIAN_POINT('',(-0.3933,-2.9267,4.81653586104654E-17));
#3942=CARTESIAN_POINT('Origin',(0.,-2.9267,0.));
#3943=CARTESIAN_POINT('',(-0.3933,-1.48,-4.81653586104654E-17));
#3944=CARTESIAN_POINT('Origin',(0.,-2.96,0.));
#3945=CARTESIAN_POINT('',(-0.32,-3.,-3.91886975727153E-17));
#3946=CARTESIAN_POINT('Origin',(0.,-3.,0.));
#3947=CARTESIAN_POINT('',(-0.36,-2.96,-4.40872847693047E-17));
#3948=CARTESIAN_POINT('Origin',(0.,-3.,0.));
#3949=CARTESIAN_POINT('Origin',(0.173205080756888,-0.8,-0.3));
#3950=CARTESIAN_POINT('',(0.346410161513775,-0.8,0.));
#3951=CARTESIAN_POINT('',(0.173205080756888,-0.8,-0.3));
#3952=CARTESIAN_POINT('',(0.346410161513775,-0.8,0.));
#3953=CARTESIAN_POINT('',(0.173205080756888,-1.28,-0.3));
#3954=CARTESIAN_POINT('',(0.173205080756888,-0.8,-0.3));
#3955=CARTESIAN_POINT('',(0.346410161513775,-1.28,0.));
#3956=CARTESIAN_POINT('',(0.346410161513775,-1.28,0.));
#3957=CARTESIAN_POINT('',(0.346410161513775,-0.8,0.));
#3958=CARTESIAN_POINT('Origin',(-0.173205080756888,-0.8,-0.3));
#3959=CARTESIAN_POINT('',(-0.173205080756888,-0.8,-0.3));
#3960=CARTESIAN_POINT('',(0.173205080756888,-0.8,-0.3));
#3961=CARTESIAN_POINT('',(-0.173205080756888,-1.28,-0.3));
#3962=CARTESIAN_POINT('',(-0.173205080756888,-0.8,-0.3));
#3963=CARTESIAN_POINT('',(0.173205080756888,-1.28,-0.3));
#3964=CARTESIAN_POINT('Origin',(-0.346410161513775,-0.8,-5.55111512312578E-17));
#3965=CARTESIAN_POINT('',(-0.346410161513775,-0.8,-4.24230095489963E-17));
#3966=CARTESIAN_POINT('',(-0.173205080756888,-0.8,-0.3));
#3967=CARTESIAN_POINT('',(-0.346410161513775,-1.28,-5.55111512312578E-17));
#3968=CARTESIAN_POINT('',(-0.346410161513775,-0.8,-4.24230095489963E-17));
#3969=CARTESIAN_POINT('',(-0.173205080756888,-1.28,-0.3));
#3970=CARTESIAN_POINT('Origin',(-0.173205080756888,-0.8,0.3));
#3971=CARTESIAN_POINT('',(-0.173205080756888,-0.8,0.3));
#3972=CARTESIAN_POINT('',(-0.346410161513775,-0.8,-4.24230095489963E-17));
#3973=CARTESIAN_POINT('',(-0.173205080756888,-1.28,0.3));
#3974=CARTESIAN_POINT('',(-0.173205080756888,-0.8,0.3));
#3975=CARTESIAN_POINT('',(-0.346410161513775,-1.28,-4.24230095489963E-17));
#3976=CARTESIAN_POINT('Origin',(0.173205080756888,-0.8,0.3));
#3977=CARTESIAN_POINT('',(0.173205080756888,-0.8,0.3));
#3978=CARTESIAN_POINT('',(-0.173205080756888,-0.8,0.3));
#3979=CARTESIAN_POINT('',(0.173205080756888,-1.28,0.3));
#3980=CARTESIAN_POINT('',(0.173205080756888,-0.8,0.3));
#3981=CARTESIAN_POINT('',(-0.173205080756888,-1.28,0.3));
#3982=CARTESIAN_POINT('Origin',(0.346410161513775,-0.8,0.));
#3983=CARTESIAN_POINT('',(0.173205080756888,-0.8,0.3));
#3984=CARTESIAN_POINT('',(0.173205080756888,-1.28,0.3));
#3985=CARTESIAN_POINT('Origin',(0.,-0.8,-5.55111512312578E-17));
#3986=CARTESIAN_POINT('Origin',(0.,-1.28,-5.55111512312578E-17));
#3987=CARTESIAN_POINT('',(0.,0.,0.));
#3988=CARTESIAN_POINT('Origin',(0.,0.9,13.75));
#3989=CARTESIAN_POINT('',(-0.165,1.,13.75));
#3990=CARTESIAN_POINT('Origin',(0.,1.,13.75));
#3991=CARTESIAN_POINT('',(-0.165,2.5,13.75));
#3992=CARTESIAN_POINT('',(-0.165,0.9,13.75));
#3993=CARTESIAN_POINT('Origin',(0.,2.5,13.75));
#3994=CARTESIAN_POINT('Origin',(0.,2.5,13.75));
#3995=CARTESIAN_POINT('Origin',(0.,6.3,13.75));
#3996=CARTESIAN_POINT('',(-1.,6.3,13.75));
#3997=CARTESIAN_POINT('Origin',(0.,6.3,13.75));
#3998=CARTESIAN_POINT('',(-0.6,6.3,13.75));
#3999=CARTESIAN_POINT('Origin',(0.,6.3,13.75));
#4000=CARTESIAN_POINT('Origin',(0.,6.3,13.75));
#4001=CARTESIAN_POINT('',(-1.,6.7,13.75));
#4002=CARTESIAN_POINT('Origin',(0.,6.7,13.75));
#4003=CARTESIAN_POINT('',(-1.,6.3,13.75));
#4004=CARTESIAN_POINT('Origin',(0.,6.7,13.75));
#4005=CARTESIAN_POINT('Origin',(0.,1.,13.75));
#4006=CARTESIAN_POINT('',(-0.6,1.,13.75));
#4007=CARTESIAN_POINT('',(-0.6,1.,13.75));
#4008=CARTESIAN_POINT('Origin',(0.,1.,13.75));
#4009=CARTESIAN_POINT('Origin',(0.,1.,13.75));
#4010=CARTESIAN_POINT('',(0.,0.,0.));
#4011=CARTESIAN_POINT('Origin',(0.,1.,13.75));
#4012=CARTESIAN_POINT('',(-0.605,1.9,13.75));
#4013=CARTESIAN_POINT('Origin',(0.,1.9,13.75));
#4014=CARTESIAN_POINT('',(-0.605,1.,13.75));
#4015=CARTESIAN_POINT('',(-0.605,1.,13.75));
#4016=CARTESIAN_POINT('Origin',(0.,1.,13.75));
#4017=CARTESIAN_POINT('Origin',(0.,1.,13.75));
#4018=CARTESIAN_POINT('',(-0.8,1.9,13.75));
#4019=CARTESIAN_POINT('Origin',(0.,1.9,13.75));
#4020=CARTESIAN_POINT('',(-0.8,1.,13.75));
#4021=CARTESIAN_POINT('',(-0.8,1.,13.75));
#4022=CARTESIAN_POINT('Origin',(0.,1.,13.75));
#4023=CARTESIAN_POINT('Origin',(0.,1.9,13.75));
#4024=CARTESIAN_POINT('Origin',(0.,1.,13.75));
#4025=CARTESIAN_POINT('',(0.,0.,0.));
#4026=CARTESIAN_POINT('Origin',(0.,4.1,13.75));
#4027=CARTESIAN_POINT('',(-0.605,5.5,13.75));
#4028=CARTESIAN_POINT('Origin',(0.,5.5,13.75));
#4029=CARTESIAN_POINT('',(-0.605,4.1,13.75));
#4030=CARTESIAN_POINT('',(-0.605,4.1,13.75));
#4031=CARTESIAN_POINT('Origin',(0.,4.1,13.75));
#4032=CARTESIAN_POINT('Origin',(0.,4.1,13.75));
#4033=CARTESIAN_POINT('',(-0.8,5.5,13.75));
#4034=CARTESIAN_POINT('Origin',(0.,5.5,13.75));
#4035=CARTESIAN_POINT('',(-0.8,4.1,13.75));
#4036=CARTESIAN_POINT('',(-0.8,4.1,13.75));
#4037=CARTESIAN_POINT('Origin',(0.,4.1,13.75));
#4038=CARTESIAN_POINT('Origin',(0.,5.5,13.75));
#4039=CARTESIAN_POINT('Origin',(0.,4.1,13.75));
#4040=CARTESIAN_POINT('',(0.,0.,0.));
#4041=CARTESIAN_POINT('Origin',(0.,2.2,4.));
#4042=CARTESIAN_POINT('',(-0.225,2.4,4.));
#4043=CARTESIAN_POINT('Origin',(0.,2.4,4.));
#4044=CARTESIAN_POINT('',(-0.225,2.2,4.));
#4045=CARTESIAN_POINT('',(-0.225,2.2,4.));
#4046=CARTESIAN_POINT('Origin',(0.,2.2,4.));
#4047=CARTESIAN_POINT('Origin',(0.,2.2,4.));
#4048=CARTESIAN_POINT('',(-0.8,2.4,4.));
#4049=CARTESIAN_POINT('Origin',(0.,2.4,4.));
#4050=CARTESIAN_POINT('',(-0.8,2.2,4.));
#4051=CARTESIAN_POINT('',(-0.8,2.2,4.));
#4052=CARTESIAN_POINT('Origin',(0.,2.2,4.));
#4053=CARTESIAN_POINT('Origin',(0.,2.4,4.));
#4054=CARTESIAN_POINT('Origin',(0.,2.2,4.));
#4055=CARTESIAN_POINT('',(0.,0.,0.));
#4056=CARTESIAN_POINT('Origin',(0.0866025403784439,-0.4,-0.15));
#4057=CARTESIAN_POINT('',(0.173205080756888,-0.4,0.));
#4058=CARTESIAN_POINT('',(0.0866025403784439,-0.4,-0.15));
#4059=CARTESIAN_POINT('',(0.173205080756888,-0.4,0.));
#4060=CARTESIAN_POINT('',(0.0866025403784439,-0.64,-0.15));
#4061=CARTESIAN_POINT('',(0.0866025403784439,-0.4,-0.15));
#4062=CARTESIAN_POINT('',(0.173205080756888,-0.64,0.));
#4063=CARTESIAN_POINT('',(0.173205080756888,-0.64,0.));
#4064=CARTESIAN_POINT('',(0.173205080756888,-0.4,0.));
#4065=CARTESIAN_POINT('Origin',(-0.0866025403784438,-0.4,-0.15));
#4066=CARTESIAN_POINT('',(-0.0866025403784438,-0.4,-0.15));
#4067=CARTESIAN_POINT('',(0.0866025403784439,-0.4,-0.15));
#4068=CARTESIAN_POINT('',(-0.0866025403784438,-0.64,-0.15));
#4069=CARTESIAN_POINT('',(-0.0866025403784438,-0.4,-0.15));
#4070=CARTESIAN_POINT('',(0.0866025403784439,-0.64,-0.15));
#4071=CARTESIAN_POINT('Origin',(-0.173205080756888,-0.4,-2.77555756156289E-17));
#4072=CARTESIAN_POINT('',(-0.173205080756888,-0.4,-2.12115047744981E-17));
#4073=CARTESIAN_POINT('',(-0.0866025403784438,-0.4,-0.15));
#4074=CARTESIAN_POINT('',(-0.173205080756888,-0.64,-2.77555756156289E-17));
#4075=CARTESIAN_POINT('',(-0.173205080756888,-0.4,-2.12115047744981E-17));
#4076=CARTESIAN_POINT('',(-0.0866025403784438,-0.64,-0.15));
#4077=CARTESIAN_POINT('Origin',(-0.0866025403784439,-0.4,0.15));
#4078=CARTESIAN_POINT('',(-0.0866025403784439,-0.4,0.15));
#4079=CARTESIAN_POINT('',(-0.173205080756888,-0.4,-2.12115047744981E-17));
#4080=CARTESIAN_POINT('',(-0.0866025403784439,-0.64,0.15));
#4081=CARTESIAN_POINT('',(-0.0866025403784439,-0.4,0.15));
#4082=CARTESIAN_POINT('',(-0.173205080756888,-0.64,-2.12115047744981E-17));
#4083=CARTESIAN_POINT('Origin',(0.0866025403784439,-0.4,0.15));
#4084=CARTESIAN_POINT('',(0.0866025403784439,-0.4,0.15));
#4085=CARTESIAN_POINT('',(-0.0866025403784439,-0.4,0.15));
#4086=CARTESIAN_POINT('',(0.0866025403784439,-0.64,0.15));
#4087=CARTESIAN_POINT('',(0.0866025403784439,-0.4,0.15));
#4088=CARTESIAN_POINT('',(-0.0866025403784439,-0.64,0.15));
#4089=CARTESIAN_POINT('Origin',(0.173205080756888,-0.4,0.));
#4090=CARTESIAN_POINT('',(0.0866025403784439,-0.4,0.15));
#4091=CARTESIAN_POINT('',(0.0866025403784439,-0.64,0.15));
#4092=CARTESIAN_POINT('Origin',(0.,-0.4,-2.77555756156289E-17));
#4093=CARTESIAN_POINT('Origin',(0.,-0.64,-2.77555756156289E-17));
#4094=CARTESIAN_POINT('Origin',(0.,-1.,0.));
#4095=CARTESIAN_POINT('',(-0.1954,-1.,2.39295984553393E-17));
#4096=CARTESIAN_POINT('Origin',(0.,-1.,0.));
#4097=CARTESIAN_POINT('Origin',(0.3,0.4,0.));
#4098=CARTESIAN_POINT('',(-0.3,0.4,-3.67394039744206E-17));
#4099=CARTESIAN_POINT('Origin',(0.,0.4,0.));
#4100=CARTESIAN_POINT('Origin',(0.,0.375,0.));
#4101=CARTESIAN_POINT('',(-0.35,0.35,-4.28626379701573E-17));
#4102=CARTESIAN_POINT('Origin',(0.,0.35,0.));
#4103=CARTESIAN_POINT('',(-0.325,0.375,-3.9801020972289E-17));
#4104=CARTESIAN_POINT('Origin',(0.,0.19,0.));
#4105=CARTESIAN_POINT('',(-0.35,0.03,-4.28626379701574E-17));
#4106=CARTESIAN_POINT('Origin',(0.,0.03,0.));
#4107=CARTESIAN_POINT('',(-0.35,0.19,-4.28626379701574E-17));
#4108=CARTESIAN_POINT('Origin',(0.,0.0149999999999999,0.));
#4109=CARTESIAN_POINT('',(-0.32,-3.29597460435593E-17,-3.91886975727153E-17));
#4110=CARTESIAN_POINT('Origin',(0.,0.,0.));
#4111=CARTESIAN_POINT('',(-0.335,0.0149999999999999,-4.10256677714363E-17));
#4112=CARTESIAN_POINT('Origin',(0.22,0.,0.));
#4113=CARTESIAN_POINT('',(-0.22,-6.93889390390723E-18,-2.69422295812418E-17));
#4114=CARTESIAN_POINT('Origin',(0.,0.,0.));
#4115=CARTESIAN_POINT('Origin',(0.,-0.02,0.));
#4116=CARTESIAN_POINT('',(-0.1954,-0.0492,2.39295984553393E-17));
#4117=CARTESIAN_POINT('Origin',(0.,-0.0492,0.));
#4118=CARTESIAN_POINT('',(-0.21,-0.02,-2.57175827820944E-17));
#4119=CARTESIAN_POINT('Origin',(0.,-0.8,0.));
#4120=CARTESIAN_POINT('',(-0.1954,-0.8,-2.39295984553393E-17));
#4121=CARTESIAN_POINT('',(0.,0.,0.));
#4122=CARTESIAN_POINT('',(0.,0.,0.));
#4123=CARTESIAN_POINT('',(0.,0.,0.));
#4124=CARTESIAN_POINT('',(21.,0.,7.));
#4125=CARTESIAN_POINT('',(-1.5,6.3,7.5));
#4126=CARTESIAN_POINT('',(-1.5,6.46,7.5));
#4127=CARTESIAN_POINT('',(1.5,6.3,7.5));
#4128=CARTESIAN_POINT('',(1.5,6.46,7.5));
#4129=CARTESIAN_POINT('',(-5.,0.,0.));
#4130=CARTESIAN_POINT('',(-5.,0.,0.));
#4131=CARTESIAN_POINT('',(-5.,0.,0.));
#4132=CARTESIAN_POINT('',(-5.,-1.4,9.75));
#4133=CARTESIAN_POINT('',(-5.,0.8,13.75));
#4134=CARTESIAN_POINT('',(5.,0.,0.));
#4135=CARTESIAN_POINT('',(5.,0.,0.));
#4136=CARTESIAN_POINT('',(5.,0.,0.));
#4137=CARTESIAN_POINT('',(5.,-1.4,9.75));
#4138=CARTESIAN_POINT('',(5.,0.8,13.75));
#4139=CARTESIAN_POINT('',(-1.5,-6.3,7.5));
#4140=CARTESIAN_POINT('',(-1.5,-6.46,7.5));
#4141=CARTESIAN_POINT('',(1.5,-6.3,7.5));
#4142=CARTESIAN_POINT('',(1.5,-6.46,7.5));
#4143=CARTESIAN_POINT('',(-5.,0.,0.));
#4144=CARTESIAN_POINT('',(-5.,0.,0.));
#4145=CARTESIAN_POINT('',(-5.,0.,0.));
#4146=CARTESIAN_POINT('',(-5.,1.4,9.75));
#4147=CARTESIAN_POINT('',(-5.,-0.8,13.75));
#4148=CARTESIAN_POINT('',(5.,0.,0.));
#4149=CARTESIAN_POINT('',(5.,0.,0.));
#4150=CARTESIAN_POINT('',(5.,0.,0.));
#4151=CARTESIAN_POINT('',(5.,1.4,9.75));
#4152=CARTESIAN_POINT('',(5.,-0.8,13.75));
#4153=CARTESIAN_POINT('',(0.,0.,0.));
#4154=CARTESIAN_POINT('',(0.,0.,0.));
#4155=CARTESIAN_POINT('Origin',(0.,0.1,4.));
#4156=CARTESIAN_POINT('',(-1.6,0.1,4.));
#4157=CARTESIAN_POINT('Origin',(0.,0.1,4.));
#4158=CARTESIAN_POINT('',(-1.6,1.2,4.));
#4159=CARTESIAN_POINT('',(-1.6,0.1,4.));
#4160=CARTESIAN_POINT('Origin',(0.,1.2,4.));
#4161=CARTESIAN_POINT('Origin',(0.,0.1,4.));
#4162=CARTESIAN_POINT('',(-0.62,0.1,4.));
#4163=CARTESIAN_POINT('Origin',(0.,0.1,4.));
#4164=CARTESIAN_POINT('Origin',(0.,-1.3,4.));
#4165=CARTESIAN_POINT('',(-1.6,-1.2,4.));
#4166=CARTESIAN_POINT('Origin',(0.,-1.2,4.));
#4167=CARTESIAN_POINT('',(-1.6,-0.0999999999999999,4.));
#4168=CARTESIAN_POINT('',(-1.6,-1.3,4.));
#4169=CARTESIAN_POINT('Origin',(0.,-0.0999999999999999,4.));
#4170=CARTESIAN_POINT('Origin',(0.,-0.0999999999999999,4.));
#4171=CARTESIAN_POINT('',(-0.62,-0.0999999999999999,4.));
#4172=CARTESIAN_POINT('Origin',(0.,-0.0999999999999999,4.));
#4173=CARTESIAN_POINT('Origin',(0.,-1.3,4.));
#4174=CARTESIAN_POINT('',(-0.62,-1.3,4.));
#4175=CARTESIAN_POINT('Origin',(0.,-1.2,4.));
#4176=CARTESIAN_POINT('',(-3.75,1.2,4.));
#4177=CARTESIAN_POINT('Origin',(0.,1.2,4.));
#4178=CARTESIAN_POINT('',(-3.75,-1.2,4.));
#4179=CARTESIAN_POINT('',(-3.75,-1.2,4.));
#4180=CARTESIAN_POINT('Origin',(0.,-1.2,4.));
#4181=CARTESIAN_POINT('Origin',(0.,1.2,4.));
#4182=CARTESIAN_POINT('Origin',(0.,-1.2,4.));
#4183=CARTESIAN_POINT('',(0.,0.,0.));
#4184=CARTESIAN_POINT('',(0.,0.,0.));
#4185=CARTESIAN_POINT('Origin',(0.,0.,0.));
#4186=CARTESIAN_POINT('',(-1.070235,-0.308121667383195,-1.31065986708547E-16));
#4187=CARTESIAN_POINT('',(-1.31065986708547E-16,-0.308121667383195,1.070235));
#4188=CARTESIAN_POINT('Origin',(0.,-0.308121667383195,0.));
#4189=CARTESIAN_POINT('Origin',(0.,-0.308121667383195,0.));
#4190=CARTESIAN_POINT('',(-1.31065986708547E-16,0.308121667383195,1.070235));
#4191=CARTESIAN_POINT('Origin',(-1.34711147906209E-16,0.,1.1));
#4192=CARTESIAN_POINT('',(-1.070235,0.308121667383195,1.31065986708547E-16));
#4193=CARTESIAN_POINT('Origin',(0.,0.308121667383195,0.));
#4194=CARTESIAN_POINT('Origin',(0.,0.308121667383195,0.));
#4195=CARTESIAN_POINT('Origin',(0.,0.,0.));
#4196=CARTESIAN_POINT('',(-1.070235,0.5,-1.31065986708547E-16));
#4197=CARTESIAN_POINT('',(-1.070235,0.,-1.31065986708547E-16));
#4198=CARTESIAN_POINT('Origin',(0.,0.5,0.));
#4199=CARTESIAN_POINT('Origin',(0.,0.,0.));
#4200=CARTESIAN_POINT('',(-0.6,-0.44,-7.34788079488412E-17));
#4201=CARTESIAN_POINT('Origin',(0.,-0.44,0.));
#4202=CARTESIAN_POINT('',(-0.6,0.44,-7.34788079488412E-17));
#4203=CARTESIAN_POINT('',(-0.6,0.,-7.34788079488412E-17));
#4204=CARTESIAN_POINT('Origin',(0.,0.44,0.));
#4205=CARTESIAN_POINT('Origin',(0.,0.47,0.));
#4206=CARTESIAN_POINT('',(-0.66,0.5,-8.08266887437253E-17));
#4207=CARTESIAN_POINT('',(-0.63,0.47,-7.71527483462832E-17));
#4208=CARTESIAN_POINT('Origin',(0.,0.5,0.));
#4209=CARTESIAN_POINT('Origin',(1.070235,0.5,0.));
#4210=CARTESIAN_POINT('Origin',(0.,0.,0.));
#4211=CARTESIAN_POINT('',(-1.070235,-0.5,-1.31065986708547E-16));
#4212=CARTESIAN_POINT('Origin',(0.,-0.5,0.));
#4213=CARTESIAN_POINT('',(-1.070235,0.,-1.31065986708547E-16));
#4214=CARTESIAN_POINT('Origin',(0.66,-0.5,0.));
#4215=CARTESIAN_POINT('',(-0.66,-0.5,-8.08266887437253E-17));
#4216=CARTESIAN_POINT('Origin',(0.,-0.5,0.));
#4217=CARTESIAN_POINT('Origin',(0.,-0.47,0.));
#4218=CARTESIAN_POINT('',(-0.63,-0.47,-7.71527483462832E-17));
#4219=CARTESIAN_POINT('',(0.,0.,0.));
#4220=CARTESIAN_POINT('Origin',(0.,0.,0.));
#4221=CARTESIAN_POINT('',(-1.129765,0.308121667383195,-1.38356309103871E-16));
#4222=CARTESIAN_POINT('',(-1.38356309103871E-16,0.308121667383195,1.129765));
#4223=CARTESIAN_POINT('Origin',(0.,0.308121667383195,0.));
#4224=CARTESIAN_POINT('Origin',(0.,0.308121667383195,0.));
#4225=CARTESIAN_POINT('',(-1.38356309103871E-16,-0.308121667383195,1.129765));
#4226=CARTESIAN_POINT('Origin',(-1.34711147906209E-16,0.,1.1));
#4227=CARTESIAN_POINT('',(-1.129765,-0.308121667383195,1.38356309103871E-16));
#4228=CARTESIAN_POINT('Origin',(0.,-0.308121667383195,0.));
#4229=CARTESIAN_POINT('Origin',(0.,-0.308121667383195,0.));
#4230=CARTESIAN_POINT('Origin',(0.,0.,0.));
#4231=CARTESIAN_POINT('',(-1.129765,-0.5,-1.38356309103871E-16));
#4232=CARTESIAN_POINT('Origin',(0.,-0.5,0.));
#4233=CARTESIAN_POINT('',(-1.129765,0.,-1.38356309103871E-16));
#4234=CARTESIAN_POINT('Origin',(1.54,0.5,0.));
#4235=CARTESIAN_POINT('',(-1.54,0.5,-1.88595607068692E-16));
#4236=CARTESIAN_POINT('Origin',(0.,0.5,0.));
#4237=CARTESIAN_POINT('',(-1.129765,0.5,-1.38356309103871E-16));
#4238=CARTESIAN_POINT('Origin',(0.,0.5,0.));
#4239=CARTESIAN_POINT('Origin',(0.,0.47,0.));
#4240=CARTESIAN_POINT('',(-1.6,0.44,-1.95943487863577E-16));
#4241=CARTESIAN_POINT('Origin',(0.,0.44,0.));
#4242=CARTESIAN_POINT('',(-1.57,0.47,-1.92269547466134E-16));
#4243=CARTESIAN_POINT('Origin',(0.,0.,0.));
#4244=CARTESIAN_POINT('',(-1.6,-0.44,-1.95943487863577E-16));
#4245=CARTESIAN_POINT('Origin',(0.,-0.44,0.));
#4246=CARTESIAN_POINT('',(-1.6,0.,-1.95943487863577E-16));
#4247=CARTESIAN_POINT('Origin',(0.,-0.47,0.));
#4248=CARTESIAN_POINT('',(-1.54,-0.5,-1.88595607068692E-16));
#4249=CARTESIAN_POINT('Origin',(0.,-0.5,0.));
#4250=CARTESIAN_POINT('',(-1.57,-0.47,-1.92269547466134E-16));
#4251=CARTESIAN_POINT('Origin',(1.129765,-0.5,0.));
#4252=CARTESIAN_POINT('Origin',(0.,0.,0.));
#4253=CARTESIAN_POINT('',(-1.129765,0.,-1.38356309103871E-16));
#4254=CARTESIAN_POINT('',(0.,0.,0.));
#4255=CARTESIAN_POINT('Origin',(1.1,0.,0.));
#4256=CARTESIAN_POINT('',(1.1,-2.23201749654651E-33,0.29765));
#4257=CARTESIAN_POINT('',(1.1,-2.23201749654651E-33,-0.29765));
#4258=CARTESIAN_POINT('Origin',(1.1,0.,0.));
#4259=CARTESIAN_POINT('Origin',(0.685838782044607,0.,-0.860014630714833));
#4260=CARTESIAN_POINT('',(0.918550922801216,-5.31350540756609E-33,-0.674432891191581));
#4261=CARTESIAN_POINT('',(0.453126641287998,8.49470414473068E-34,-1.04559637023808));
#4262=CARTESIAN_POINT('Origin',(0.685838782044607,0.,-0.860014630714833));
#4263=CARTESIAN_POINT('Origin',(-0.244773027351946,0.,-1.07242070340001));
#4264=CARTESIAN_POINT('',(0.0454142657089739,-2.23201749654651E-33,-1.1386540593921));
#4265=CARTESIAN_POINT('',(-0.534960320412865,-2.23201749654651E-33,-1.00618734740791));
#4266=CARTESIAN_POINT('Origin',(-0.244773027351946,0.,-1.07242070340001));
#4267=CARTESIAN_POINT('Origin',(-0.991065754692661,0.,-0.477272113029314));
#4268=CARTESIAN_POINT('',(-0.86192025974432,8.49470414473067E-34,-0.745445496560469));
#4269=CARTESIAN_POINT('',(-1.120211249641,-5.31350540756609E-33,-0.209098729498159));
#4270=CARTESIAN_POINT('Origin',(-0.991065754692661,0.,-0.477272113029314));
#4271=CARTESIAN_POINT('Origin',(-0.991065754692661,0.,0.477272113029314));
#4272=CARTESIAN_POINT('',(-1.120211249641,-2.23201749654651E-33,0.209098729498159));
#4273=CARTESIAN_POINT('',(-0.86192025974432,-2.23201749654651E-33,0.745445496560469));
#4274=CARTESIAN_POINT('Origin',(-0.991065754692661,0.,0.477272113029314));
#4275=CARTESIAN_POINT('Origin',(-0.244773027351946,0.,1.07242070340001));
#4276=CARTESIAN_POINT('',(-0.534960320412866,-2.23201749654651E-33,1.00618734740791));
#4277=CARTESIAN_POINT('',(0.0454142657089737,-2.23201749654651E-33,1.1386540593921));
#4278=CARTESIAN_POINT('Origin',(-0.244773027351946,0.,1.07242070340001));
#4279=CARTESIAN_POINT('Origin',(0.685838782044607,0.,0.860014630714833));
#4280=CARTESIAN_POINT('',(0.453126641287998,-2.23201749654651E-33,1.04559637023808));
#4281=CARTESIAN_POINT('',(0.918550922801216,-2.23201749654651E-33,0.674432891191581));
#4282=CARTESIAN_POINT('Origin',(0.685838782044607,0.,0.860014630714833));
#4283=CARTESIAN_POINT('',(0.,0.,0.));
#4284=CARTESIAN_POINT('Origin',(0.685838782044607,0.,0.860014630714833));
#4285=CARTESIAN_POINT('',(0.413083465285518,-0.05953,0.993751811093549));
#4286=CARTESIAN_POINT('',(0.876916659919095,-0.05953,0.623857181492959));
#4287=CARTESIAN_POINT('Ctrl Pts',(0.413083465285518,-0.05953,0.993751811093549));
#4288=CARTESIAN_POINT('Ctrl Pts',(0.419070565453383,-0.0925528133349865,
0.991263089003441));
#4289=CARTESIAN_POINT('Ctrl Pts',(0.430199341854858,-0.124911173756694,
0.986608710139579));
#4290=CARTESIAN_POINT('Ctrl Pts',(0.457978755888596,-0.177924977804098,
0.973971221090534));
#4291=CARTESIAN_POINT('Ctrl Pts',(0.473077587363685,-0.199697230012983,
0.966820759530997));
#4292=CARTESIAN_POINT('Ctrl Pts',(0.507057380724533,-0.237895043532788,
0.949440676105255));
#4293=CARTESIAN_POINT('Ctrl Pts',(0.525933334162555,-0.254319232363049,
0.939198248544428));
#4294=CARTESIAN_POINT('Ctrl Pts',(0.564362943424238,-0.28018331644634,0.916597376014514));
#4295=CARTESIAN_POINT('Ctrl Pts',(0.585840553788742,-0.29104845371857,0.903141581680914));
#4296=CARTESIAN_POINT('Ctrl Pts',(0.629305439856167,-0.30527573347708,0.873412008702649));
#4297=CARTESIAN_POINT('Ctrl Pts',(0.651278921914856,-0.308638795020976,
0.857118508332695));
#4298=CARTESIAN_POINT('Ctrl Pts',(0.690705563850638,-0.308638795020976,
0.825676810575914));
#4299=CARTESIAN_POINT('Ctrl Pts',(0.711480111898423,-0.30527573347708,0.807879894508811));
#4300=CARTESIAN_POINT('Ctrl Pts',(0.750136149454208,-0.29104845371857,0.772120216227122));
#4301=CARTESIAN_POINT('Ctrl Pts',(0.768033796848072,-0.28018331644634,0.754175290318038));
#4302=CARTESIAN_POINT('Ctrl Pts',(0.798619410861634,-0.254319232363049,
0.721738358858166));
#4303=CARTESIAN_POINT('Ctrl Pts',(0.812805334167529,-0.237895043532788,
0.705614819529209));
#4304=CARTESIAN_POINT('Ctrl Pts',(0.837310877969633,-0.199697230012983,
0.676354402927683));
#4305=CARTESIAN_POINT('Ctrl Pts',(0.847641868610495,-0.177924977804098,
0.663225258065736));
#4306=CARTESIAN_POINT('Ctrl Pts',(0.866144010579847,-0.124911173756694,
0.638954437806245));
#4307=CARTESIAN_POINT('Ctrl Pts',(0.873158080166742,-0.0925528133349865,
0.62914037979579));
#4308=CARTESIAN_POINT('Ctrl Pts',(0.876916659919095,-0.05953,0.623857181492959));
#4309=CARTESIAN_POINT('',(0.437601487681057,-0.05953,1.03511272300331));
#4310=CARTESIAN_POINT('Origin',(0.685838782044607,-0.05953,0.860014630714833));
#4311=CARTESIAN_POINT('',(0.911784794170997,-0.05953,0.656964154625313));
#4312=CARTESIAN_POINT('Ctrl Pts',(0.911784794170998,-0.0595300000000001,
0.656964154625312));
#4313=CARTESIAN_POINT('Ctrl Pts',(0.909827729890942,-0.0762225747374255,
0.659680317203144));
#4314=CARTESIAN_POINT('Ctrl Pts',(0.907004864562642,-0.0928409665394228,
0.663576540841106));
#4315=CARTESIAN_POINT('Ctrl Pts',(0.895234408667242,-0.144299303100741,
0.679480524217551));
#4316=CARTESIAN_POINT('Ctrl Pts',(0.882797231409153,-0.177024326825049,
0.695831250979106));
#4317=CARTESIAN_POINT('Ctrl Pts',(0.854332839576145,-0.227269801620064,
0.73042219438957));
#4318=CARTESIAN_POINT('Ctrl Pts',(0.834863020612702,-0.251265615809407,
0.752807465209441));
#4319=CARTESIAN_POINT('Ctrl Pts',(0.800439809856111,-0.279889827963178,
0.789147407129766));
#4320=CARTESIAN_POINT('Ctrl Pts',(0.781998747691871,-0.290879136862659,
0.80756613568454));
#4321=CARTESIAN_POINT('Ctrl Pts',(0.742239891936898,-0.305251990234487,
0.844254137480382));
#4322=CARTESIAN_POINT('Ctrl Pts',(0.720906778729541,-0.308638795020976,
0.862505527716294));
#4323=CARTESIAN_POINT('Ctrl Pts',(0.680463863683392,-0.308638795020976,
0.894757676234429));
#4324=CARTESIAN_POINT('Ctrl Pts',(0.657923009631182,-0.305251990234488,
0.91149460735272));
#4325=CARTESIAN_POINT('Ctrl Pts',(0.613307674922609,-0.290879136862659,
0.942092777160053));
#4326=CARTESIAN_POINT('Ctrl Pts',(0.591247219971725,-0.279889827963178,
0.955972930713954));
#4327=CARTESIAN_POINT('Ctrl Pts',(0.548158511259202,-0.251265615809407,
0.981446681891443));
#4328=CARTESIAN_POINT('Ctrl Pts',(0.522002043615455,-0.227269801620063,
0.995447160474328));
#4329=CARTESIAN_POINT('Ctrl Pts',(0.481944444320713,-0.177024326825049,
1.01550068154148));
#4330=CARTESIAN_POINT('Ctrl Pts',(0.463236132117164,-0.14429930310074,1.0239876538093));
#4331=CARTESIAN_POINT('Ctrl Pts',(0.445111721969657,-0.0928409665394226,
1.03192403056628));
#4332=CARTESIAN_POINT('Ctrl Pts',(0.440685038163619,-0.0762225747374254,
1.03380912944435));
#4333=CARTESIAN_POINT('Ctrl Pts',(0.437601487681056,-0.05953,1.03511272300331));
#4334=CARTESIAN_POINT('Origin',(0.685838782044607,-0.05953,0.860014630714833));
#4335=CARTESIAN_POINT('Origin',(0.,-0.208355,0.));
#4336=CARTESIAN_POINT('',(0.0548532617164168,-0.05953,1.12247250791415));
#4337=CARTESIAN_POINT('Origin',(0.,-0.05953,0.));
#4338=CARTESIAN_POINT('',(-0.536443649899848,-0.05953,0.987512846410683));
#4339=CARTESIAN_POINT('Ctrl Pts',(0.0548532617164173,-0.0595300000000001,
1.12247250791414));
#4340=CARTESIAN_POINT('Ctrl Pts',(0.05150947068137,-0.0762225747374254,
1.12263591311425));
#4341=CARTESIAN_POINT('Ctrl Pts',(0.0467032526342597,-0.0928409665394227,
1.12285816383385));
#4342=CARTESIAN_POINT('Ctrl Pts',(0.0269302585198975,-0.144299303100741,
1.12357162229597));
#4343=CARTESIAN_POINT('Ctrl Pts',(0.006392292392153,-0.177024326825049,
1.12404235695137));
#4344=CARTESIAN_POINT('Ctrl Pts',(-0.0383992541984087,-0.227269801620063,
1.12335509974011));
#4345=CARTESIAN_POINT('Ctrl Pts',(-0.0680399972366993,-0.251265615809407,
1.12208997038458));
#4346=CARTESIAN_POINT('Ctrl Pts',(-0.117914228755037,-0.279889827963178,
1.1178344036749));
#4347=CARTESIAN_POINT('Ctrl Pts',(-0.14381238480104,-0.290879136862659,
1.11490049012186));
#4348=CARTESIAN_POINT('Ctrl Pts',(-0.19728546073067,-0.305251990234488,
1.10669035995599));
#4349=CARTESIAN_POINT('Ctrl Pts',(-0.224855950742601,-0.308638795020976,
1.10139101611326));
#4350=CARTESIAN_POINT('Ctrl Pts',(-0.275287440920027,-0.308638795020976,
1.0898803575765));
#4351=CARTESIAN_POINT('Ctrl Pts',(-0.302426893214945,-0.305251990234488,
1.08269251410343));
#4352=CARTESIAN_POINT('Ctrl Pts',(-0.35416671187353,-0.290879136862659,
1.06688848765783));
#4353=CARTESIAN_POINT('Ctrl Pts',(-0.3787731215897,-0.279889827963178,1.05829506364875));
#4354=CARTESIAN_POINT('Ctrl Pts',(-0.425554672694338,-0.251265615809407,
1.04048957871266));
#4355=CARTESIAN_POINT('Ctrl Pts',(-0.452808978448581,-0.227269801620063,
1.02876878445619));
#4356=CARTESIAN_POINT('Ctrl Pts',(-0.493462957200432,-0.177024326825049,
1.0099536580922));
#4357=CARTESIAN_POINT('Ctrl Pts',(-0.511762781179148,-0.14429930310074,
1.00061845128527));
#4358=CARTESIAN_POINT('Ctrl Pts',(-0.529268075276157,-0.0928409665394226,
0.991396466802468));
#4359=CARTESIAN_POINT('Ctrl Pts',(-0.533501897135713,-0.0762225747374254,
0.989110885965947));
#4360=CARTESIAN_POINT('Ctrl Pts',(-0.536443649899848,-0.0595300000000001,
0.987512846410683));
#4361=CARTESIAN_POINT('',(-0.843383895613249,-0.05953,0.742736168477219));
#4362=CARTESIAN_POINT('Origin',(0.,-0.05953,0.));
#4363=CARTESIAN_POINT('',(-1.10653577764992,-0.05953,0.196295654879792));
#4364=CARTESIAN_POINT('Ctrl Pts',(-0.843383895613249,-0.0595300000000001,
0.742736168477219));
#4365=CARTESIAN_POINT('Ctrl Pts',(-0.84559647055299,-0.0762225747374255,
0.740223768851062));
#4366=CARTESIAN_POINT('Ctrl Pts',(-0.848766861100456,-0.0928409665394227,
0.736604687327351));
#4367=CARTESIAN_POINT('Ctrl Pts',(-0.861652925570091,-0.144299303100741,
0.721590372101268));
#4368=CARTESIAN_POINT('Ctrl Pts',(-0.87482617317514,-0.177024326825049,
0.705826641853758));
#4369=CARTESIAN_POINT('Ctrl Pts',(-0.902215926359523,-0.227269801620063,
0.670378702718353));
#4370=CARTESIAN_POINT('Ctrl Pts',(-0.919707509403859,-0.251265615809407,
0.646415841396062));
#4371=CARTESIAN_POINT('Ctrl Pts',(-0.947476448101718,-0.279889827963178,
0.604769294586516));
#4372=CARTESIAN_POINT('Ctrl Pts',(-0.961329858300736,-0.290879136862659,
0.582692035672022));
#4373=CARTESIAN_POINT('Ctrl Pts',(-0.988250837578047,-0.305251990234488,
0.535766169015486));
#4374=CARTESIAN_POINT('Ctrl Pts',(-1.00129756308006,-0.308638795020976,
0.510906605094603));
#4375=CARTESIAN_POINT('Ctrl Pts',(-1.02374168767024,-0.308638795020976,
0.46430090015576));
#4376=CARTESIAN_POINT('Ctrl Pts',(-1.03504317708586,-0.305251990234488,
0.438600874831839));
#4377=CARTESIAN_POINT('Ctrl Pts',(-1.05494634094458,-0.290879136862659,
0.388295406390235));
#4378=CARTESIAN_POINT('Ctrl Pts',(-1.06356957703048,-0.279889827963178,
0.363699428370917));
#4379=CARTESIAN_POINT('Ctrl Pts',(-1.0788165083757,-0.251265615809407,0.316022600643821));
#4380=CARTESIAN_POINT('Ctrl Pts',(-1.08664560412098,-0.227269801620063,
0.287406530683752));
#4381=CARTESIAN_POINT('Ctrl Pts',(-1.09728268713976,-0.177024326825049,
0.243890930799337));
#4382=CARTESIAN_POINT('Ctrl Pts',(-1.10139388218929,-0.144299303100741,
0.22376314604679));
#4383=CARTESIAN_POINT('Ctrl Pts',(-1.10509821673782,-0.0928409665394227,
0.204327142733961));
#4384=CARTESIAN_POINT('Ctrl Pts',(-1.10595102243643,-0.0762225747374254,
0.199591971170104));
#4385=CARTESIAN_POINT('Ctrl Pts',(-1.10653577764992,-0.0595300000000001,
0.196295654879792));
#4386=CARTESIAN_POINT('',(-1.123812,-0.05953,1.37627276864339E-16));
#4387=CARTESIAN_POINT('Origin',(0.,-0.05953,0.));
#4388=CARTESIAN_POINT('',(-1.123812,-0.35718,1.37627276864339E-16));
#4389=CARTESIAN_POINT('',(-1.123812,-0.208355,1.37627276864339E-16));
#4390=CARTESIAN_POINT('Origin',(0.,-0.35718,0.));
#4391=CARTESIAN_POINT('',(-1.10653577764992,-0.05953,-0.196295654879793));
#4392=CARTESIAN_POINT('Origin',(0.,-0.05953,0.));
#4393=CARTESIAN_POINT('',(-0.843383895613249,-0.05953,-0.742736168477219));
#4394=CARTESIAN_POINT('Ctrl Pts',(-1.10653577764992,-0.0595300000000001,
-0.196295654879792));
#4395=CARTESIAN_POINT('Ctrl Pts',(-1.10595102243643,-0.0762225747374255,
-0.199591971170104));
#4396=CARTESIAN_POINT('Ctrl Pts',(-1.10509821673782,-0.0928409665394228,
-0.204327142733962));
#4397=CARTESIAN_POINT('Ctrl Pts',(-1.10139388218929,-0.144299303100741,
-0.22376314604679));
#4398=CARTESIAN_POINT('Ctrl Pts',(-1.09728268713976,-0.177024326825049,
-0.243890930799338));
#4399=CARTESIAN_POINT('Ctrl Pts',(-1.08664560412098,-0.227269801620063,
-0.287406530683753));
#4400=CARTESIAN_POINT('Ctrl Pts',(-1.0788165083757,-0.251265615809407,-0.316022600643821));
#4401=CARTESIAN_POINT('Ctrl Pts',(-1.06356957703048,-0.279889827963178,
-0.363699428370918));
#4402=CARTESIAN_POINT('Ctrl Pts',(-1.05494634094458,-0.290879136862659,
-0.388295406390235));
#4403=CARTESIAN_POINT('Ctrl Pts',(-1.03504317708586,-0.305251990234488,
-0.438600874831839));
#4404=CARTESIAN_POINT('Ctrl Pts',(-1.02374168767024,-0.308638795020976,
-0.46430090015576));
#4405=CARTESIAN_POINT('Ctrl Pts',(-1.00129756308006,-0.308638795020976,
-0.510906605094603));
#4406=CARTESIAN_POINT('Ctrl Pts',(-0.988250837578047,-0.305251990234488,
-0.535766169015486));
#4407=CARTESIAN_POINT('Ctrl Pts',(-0.961329858300736,-0.290879136862659,
-0.582692035672022));
#4408=CARTESIAN_POINT('Ctrl Pts',(-0.947476448101718,-0.279889827963178,
-0.604769294586516));
#4409=CARTESIAN_POINT('Ctrl Pts',(-0.919707509403859,-0.251265615809407,
-0.646415841396062));
#4410=CARTESIAN_POINT('Ctrl Pts',(-0.902215926359523,-0.227269801620064,
-0.670378702718353));
#4411=CARTESIAN_POINT('Ctrl Pts',(-0.87482617317514,-0.177024326825049,
-0.705826641853758));
#4412=CARTESIAN_POINT('Ctrl Pts',(-0.861652925570091,-0.144299303100741,
-0.721590372101268));
#4413=CARTESIAN_POINT('Ctrl Pts',(-0.848766861100456,-0.0928409665394229,
-0.736604687327351));
#4414=CARTESIAN_POINT('Ctrl Pts',(-0.84559647055299,-0.0762225747374255,
-0.740223768851063));
#4415=CARTESIAN_POINT('Ctrl Pts',(-0.843383895613249,-0.0595300000000001,
-0.742736168477219));
#4416=CARTESIAN_POINT('',(-0.536443649899847,-0.05953,-0.987512846410683));
#4417=CARTESIAN_POINT('Origin',(0.,-0.05953,0.));
#4418=CARTESIAN_POINT('',(0.0548532617164172,-0.05953,-1.12247250791415));
#4419=CARTESIAN_POINT('Ctrl Pts',(-0.536443649899848,-0.0595300000000001,
-0.987512846410683));
#4420=CARTESIAN_POINT('Ctrl Pts',(-0.533501897135712,-0.0762225747374254,
-0.989110885965947));
#4421=CARTESIAN_POINT('Ctrl Pts',(-0.529268075276156,-0.0928409665394227,
-0.991396466802469));
#4422=CARTESIAN_POINT('Ctrl Pts',(-0.511762781179147,-0.144299303100741,
-1.00061845128527));
#4423=CARTESIAN_POINT('Ctrl Pts',(-0.493462957200432,-0.177024326825049,
-1.0099536580922));
#4424=CARTESIAN_POINT('Ctrl Pts',(-0.45280897844858,-0.227269801620063,
-1.02876878445619));
#4425=CARTESIAN_POINT('Ctrl Pts',(-0.425554672694337,-0.251265615809407,
-1.04048957871266));
#4426=CARTESIAN_POINT('Ctrl Pts',(-0.3787731215897,-0.279889827963178,-1.05829506364875));
#4427=CARTESIAN_POINT('Ctrl Pts',(-0.354166711873529,-0.290879136862659,
-1.06688848765783));
#4428=CARTESIAN_POINT('Ctrl Pts',(-0.302426893214944,-0.305251990234488,
-1.08269251410343));
#4429=CARTESIAN_POINT('Ctrl Pts',(-0.275287440920027,-0.308638795020976,
-1.0898803575765));
#4430=CARTESIAN_POINT('Ctrl Pts',(-0.224855950742601,-0.308638795020976,
-1.10139101611326));
#4431=CARTESIAN_POINT('Ctrl Pts',(-0.19728546073067,-0.305251990234488,
-1.10669035995599));
#4432=CARTESIAN_POINT('Ctrl Pts',(-0.143812384801039,-0.290879136862659,
-1.11490049012186));
#4433=CARTESIAN_POINT('Ctrl Pts',(-0.117914228755037,-0.279889827963178,
-1.1178344036749));
#4434=CARTESIAN_POINT('Ctrl Pts',(-0.0680399972366989,-0.251265615809407,
-1.12208997038458));
#4435=CARTESIAN_POINT('Ctrl Pts',(-0.0383992541984084,-0.227269801620063,
-1.12335509974011));
#4436=CARTESIAN_POINT('Ctrl Pts',(0.00639229239215326,-0.177024326825049,
-1.12404235695137));
#4437=CARTESIAN_POINT('Ctrl Pts',(0.0269302585198977,-0.144299303100741,
-1.12357162229597));
#4438=CARTESIAN_POINT('Ctrl Pts',(0.04670325263426,-0.0928409665394228,
-1.12285816383385));
#4439=CARTESIAN_POINT('Ctrl Pts',(0.0515094706813703,-0.0762225747374255,
-1.12263591311425));
#4440=CARTESIAN_POINT('Ctrl Pts',(0.0548532617164176,-0.0595300000000001,
-1.12247250791414));
#4441=CARTESIAN_POINT('',(0.437601487681057,-0.05953,-1.03511272300331));
#4442=CARTESIAN_POINT('Origin',(0.,-0.05953,0.));
#4443=CARTESIAN_POINT('',(0.911784794170997,-0.05953,-0.656964154625313));
#4444=CARTESIAN_POINT('Ctrl Pts',(0.437601487681056,-0.0595300000000001,
-1.03511272300331));
#4445=CARTESIAN_POINT('Ctrl Pts',(0.440685038163619,-0.0762225747374255,
-1.03380912944435));
#4446=CARTESIAN_POINT('Ctrl Pts',(0.445111721969657,-0.0928409665394228,
-1.03192403056628));
#4447=CARTESIAN_POINT('Ctrl Pts',(0.463236132117164,-0.144299303100741,
-1.0239876538093));
#4448=CARTESIAN_POINT('Ctrl Pts',(0.481944444320713,-0.177024326825049,
-1.01550068154148));
#4449=CARTESIAN_POINT('Ctrl Pts',(0.522002043615455,-0.227269801620064,
-0.995447160474328));
#4450=CARTESIAN_POINT('Ctrl Pts',(0.548158511259203,-0.251265615809407,
-0.981446681891443));
#4451=CARTESIAN_POINT('Ctrl Pts',(0.591247219971725,-0.279889827963178,
-0.955972930713954));
#4452=CARTESIAN_POINT('Ctrl Pts',(0.613307674922609,-0.290879136862659,
-0.942092777160053));
#4453=CARTESIAN_POINT('Ctrl Pts',(0.657923009631182,-0.305251990234487,
-0.91149460735272));
#4454=CARTESIAN_POINT('Ctrl Pts',(0.680463863683393,-0.308638795020976,
-0.894757676234429));
#4455=CARTESIAN_POINT('Ctrl Pts',(0.720906778729542,-0.308638795020976,
-0.862505527716294));
#4456=CARTESIAN_POINT('Ctrl Pts',(0.742239891936899,-0.305251990234488,
-0.844254137480381));
#4457=CARTESIAN_POINT('Ctrl Pts',(0.781998747691872,-0.290879136862659,
-0.80756613568454));
#4458=CARTESIAN_POINT('Ctrl Pts',(0.800439809856112,-0.279889827963178,
-0.789147407129765));
#4459=CARTESIAN_POINT('Ctrl Pts',(0.834863020612702,-0.251265615809407,
-0.752807465209441));
#4460=CARTESIAN_POINT('Ctrl Pts',(0.854332839576145,-0.227269801620064,
-0.73042219438957));
#4461=CARTESIAN_POINT('Ctrl Pts',(0.882797231409153,-0.177024326825049,
-0.695831250979106));
#4462=CARTESIAN_POINT('Ctrl Pts',(0.895234408667242,-0.144299303100741,
-0.679480524217551));
#4463=CARTESIAN_POINT('Ctrl Pts',(0.907004864562642,-0.0928409665394228,
-0.663576540841106));
#4464=CARTESIAN_POINT('Ctrl Pts',(0.909827729890942,-0.0762225747374256,
-0.659680317203144));
#4465=CARTESIAN_POINT('Ctrl Pts',(0.911784794170998,-0.0595300000000001,
-0.656964154625312));
#4466=CARTESIAN_POINT('',(1.08212377959455,-0.05953,-0.303251606722892));
#4467=CARTESIAN_POINT('Origin',(0.,-0.05953,0.));
#4468=CARTESIAN_POINT('',(1.08212377959455,-0.05953,0.303251606722892));
#4469=CARTESIAN_POINT('Ctrl Pts',(1.08212377959455,-0.0595300000000001,
-0.303251606722892));
#4470=CARTESIAN_POINT('Ctrl Pts',(1.0830271513892,-0.0762225747374255,-0.300028012588062));
#4471=CARTESIAN_POINT('Ctrl Pts',(1.08431331394788,-0.0928409665394228,
-0.2953917518996));
#4472=CARTESIAN_POINT('Ctrl Pts',(1.08940878963422,-0.144299303100741,-0.276273267473431));
#4473=CARTESIAN_POINT('Ctrl Pts',(1.09443784939331,-0.177024326825049,-0.256354979351213));
#4474=CARTESIAN_POINT('Ctrl Pts',(1.10373487993589,-0.227269801620064,-0.212533521233765));
#4475=CARTESIAN_POINT('Ctrl Pts',(1.10909715583869,-0.251265615809407,-0.183354415742157));
#4476=CARTESIAN_POINT('Ctrl Pts',(1.1160463456491,-0.279889827963178,-0.133783682657561));
#4477=CARTESIAN_POINT('Ctrl Pts',(1.11894887330541,-0.290879136862659,-0.107881990270302));
#4478=CARTESIAN_POINT('Ctrl Pts',(1.12284346704144,-0.305251990234488,-0.0539226701638766));
#4479=CARTESIAN_POINT('Ctrl Pts',(1.123812,-0.308638795020976,-0.025864214957475));
#4480=CARTESIAN_POINT('Ctrl Pts',(1.123812,-0.308638795020976,0.025864214957475));
#4481=CARTESIAN_POINT('Ctrl Pts',(1.12284346704144,-0.305251990234488,0.0539226701638766));
#4482=CARTESIAN_POINT('Ctrl Pts',(1.11894887330541,-0.290879136862659,0.107881990270302));
#4483=CARTESIAN_POINT('Ctrl Pts',(1.1160463456491,-0.279889827963178,0.133783682657561));
#4484=CARTESIAN_POINT('Ctrl Pts',(1.10909715583869,-0.251265615809407,0.183354415742157));
#4485=CARTESIAN_POINT('Ctrl Pts',(1.10373487993589,-0.227269801620064,0.212533521233765));
#4486=CARTESIAN_POINT('Ctrl Pts',(1.09443784939331,-0.177024326825049,0.256354979351213));
#4487=CARTESIAN_POINT('Ctrl Pts',(1.08940878963422,-0.144299303100741,0.276273267473431));
#4488=CARTESIAN_POINT('Ctrl Pts',(1.08431331394788,-0.0928409665394228,
0.2953917518996));
#4489=CARTESIAN_POINT('Ctrl Pts',(1.0830271513892,-0.0762225747374255,0.300028012588062));
#4490=CARTESIAN_POINT('Ctrl Pts',(1.08212377959455,-0.0595300000000001,
0.303251606722892));
#4491=CARTESIAN_POINT('Origin',(0.,-0.05953,0.));
#4492=CARTESIAN_POINT('Origin',(0.,-0.05953,0.));
#4493=CARTESIAN_POINT('',(0.0589974094846122,-0.05953,1.07456964270265));
#4494=CARTESIAN_POINT('Origin',(0.,-0.05953,0.));
#4495=CARTESIAN_POINT('Origin',(-0.244773027351946,-0.05953,1.07242070340001));
#4496=CARTESIAN_POINT('Origin',(-0.244773027351946,0.,1.07242070340001));
#4497=CARTESIAN_POINT('',(-0.519393123750572,-0.05953,0.942555777842682));
#4498=CARTESIAN_POINT('Ctrl Pts',(-0.519393123750572,-0.05953,0.942555777842682));
#4499=CARTESIAN_POINT('Ctrl Pts',(-0.513714466572041,-0.0925528133349865,
0.945684988399766));
#4500=CARTESIAN_POINT('Ctrl Pts',(-0.503136848051455,-0.124911173756694,
0.951483858396181));
#4501=CARTESIAN_POINT('Ctrl Pts',(-0.47593627990192,-0.177924977804098,
0.965323333309091));
#4502=CARTESIAN_POINT('Ctrl Pts',(-0.460931856495794,-0.199697230012983,
0.972669835243841));
#4503=CARTESIAN_POINT('Ctrl Pts',(-0.426157505475872,-0.237895043532788,
0.988400002689705));
#4504=CARTESIAN_POINT('Ctrl Pts',(-0.406380688682952,-0.254319232363049,
0.996771768218699));
#4505=CARTESIAN_POINT('Ctrl Pts',(-0.364750145543744,-0.28018331644634,
1.01272583306292));
#4506=CARTESIAN_POINT('Ctrl Pts',(-0.340838910881557,-0.29104845371857,
1.02112815447116));
#4507=CARTESIAN_POINT('Ctrl Pts',(-0.290495481564827,-0.30527573347708,
1.036574285215));
#4508=CARTESIAN_POINT('Ctrl Pts',(-0.264056468041074,-0.308638795020976,
1.04359501395068));
#4509=CARTESIAN_POINT('Ctrl Pts',(-0.214892249704082,-0.308638795020976,
1.05481642595959));
#4510=CARTESIAN_POINT('Ctrl Pts',(-0.188025341585962,-0.30527573347708,
1.05996242598502));
#4511=CARTESIAN_POINT('Ctrl Pts',(-0.135965654106109,-0.29104845371857,
1.06788913840721));
#4512=CARTESIAN_POINT('Ctrl Pts',(-0.110776745452494,-0.28018331644634,
1.07069360430242));
#4513=CARTESIAN_POINT('Ctrl Pts',(-0.0663467128214646,-0.254319232363049,
1.07438230428002));
#4514=CARTESIAN_POINT('Ctrl Pts',(-0.0448960436540983,-0.237895043532788,
1.07542044338697));
#4515=CARTESIAN_POINT('Ctrl Pts',(-0.00674037211528124,-0.199697230012983,
1.07633607767727));
#4516=CARTESIAN_POINT('Ctrl Pts',(0.00996567398334777,-0.177924977804098,
1.07622728347683));
#4517=CARTESIAN_POINT('Ctrl Pts',(0.0404772621979741,-0.124911173756694,
1.07556023164702));
#4518=CARTESIAN_POINT('Ctrl Pts',(0.0525234025782719,-0.0925528133349865,
1.07492508698591));
#4519=CARTESIAN_POINT('Ctrl Pts',(0.0589974094846124,-0.05953,1.07456964270265));
#4520=CARTESIAN_POINT('Origin',(-0.244773027351946,-0.05953,1.07242070340001));
#4521=CARTESIAN_POINT('Origin',(0.,-0.05953,0.));
#4522=CARTESIAN_POINT('',(-0.803348093619616,-0.05953,0.716109245731214));
#4523=CARTESIAN_POINT('Origin',(0.,-0.05953,0.));
#4524=CARTESIAN_POINT('Origin',(-0.991065754692661,-0.05953,0.477272113029314));
#4525=CARTESIAN_POINT('Origin',(-0.991065754692661,0.,0.477272113029314));
#4526=CARTESIAN_POINT('',(-1.06075609691358,-0.05953,0.181596019242328));
#4527=CARTESIAN_POINT('Ctrl Pts',(-1.06075609691358,-0.05953,0.181596019242328));
#4528=CARTESIAN_POINT('Ctrl Pts',(-1.05966202740332,-0.0925528133349865,
0.187986803072856));
#4529=CARTESIAN_POINT('Ctrl Pts',(-1.05760072925372,-0.124911173756694,
0.199872254546857));
#4530=CARTESIAN_POINT('Ctrl Pts',(-1.05146158959546,-0.177924977804098,
0.22976728653846));
#4531=CARTESIAN_POINT('Ctrl Pts',(-1.04785021111757,-0.199697230012983,
0.246078686169301));
#4532=CARTESIAN_POINT('Ctrl Pts',(-1.03846709802406,-0.237895043532788,
0.283073967563097));
#4533=CARTESIAN_POINT('Ctrl Pts',(-1.03268176429485,-0.254319232363049,
0.303755815985685));
#4534=CARTESIAN_POINT('Ctrl Pts',(-1.01919893537026,-0.28018331644634,0.346251081972725));
#4535=CARTESIAN_POINT('Ctrl Pts',(-1.01085972381132,-0.29104845371857,0.370184399726282));
#4536=CARTESIAN_POINT('Ctrl Pts',(-0.99154738033959,-0.30527573347708,0.419174982698463));
#4537=CARTESIAN_POINT('Ctrl Pts',(-0.980551951791748,-0.308638795020976,
0.444223188605045));
#4538=CARTESIAN_POINT('Ctrl Pts',(-0.958671816228589,-0.308638795020976,
0.489657758261848));
#4539=CARTESIAN_POINT('Ctrl Pts',(-0.945943877838127,-0.30527573347708,
0.51387163140139));
#4540=CARTESIAN_POINT('Ctrl Pts',(-0.91968254693063,-0.29104845371857,0.559515758398093));
#4541=CARTESIAN_POINT('Ctrl Pts',(-0.906170138993533,-0.28018331644634,
0.580957796077825));
#4542=CARTESIAN_POINT('Ctrl Pts',(-0.8813524085237,-0.254319232363049,0.617994461173994));
#4543=CARTESIAN_POINT('Ctrl Pts',(-0.868789784891799,-0.237895043532788,
0.635412538795143));
#4544=CARTESIAN_POINT('Ctrl Pts',(-0.845715984518854,-0.199697230012983,
0.66581473268113));
#4545=CARTESIAN_POINT('Ctrl Pts',(-0.835214876415962,-0.177924977804098,
0.678808213394124));
#4546=CARTESIAN_POINT('Ctrl Pts',(-0.815669690204649,-0.124911173756694,
0.702247233627224));
#4547=CARTESIAN_POINT('Ctrl Pts',(-0.807662468433796,-0.0925528133349865,
0.711269279199861));
#4548=CARTESIAN_POINT('Ctrl Pts',(-0.803348093619616,-0.05953,0.716109245731214));
#4549=CARTESIAN_POINT('Origin',(-0.991065754692661,-0.05953,0.477272113029314));
#4550=CARTESIAN_POINT('Origin',(0.,-0.05953,0.));
#4551=CARTESIAN_POINT('',(-1.076188,-0.05953,1.31795018948079E-16));
#4552=CARTESIAN_POINT('Origin',(0.,-0.05953,0.));
#4553=CARTESIAN_POINT('',(-1.06075609691358,-0.05953,-0.181596019242328));
#4554=CARTESIAN_POINT('Origin',(0.,-0.05953,0.));
#4555=CARTESIAN_POINT('Origin',(-0.991065754692661,-0.05953,-0.477272113029314));
#4556=CARTESIAN_POINT('Origin',(-0.991065754692661,0.,-0.477272113029314));
#4557=CARTESIAN_POINT('',(-0.803348093619616,-0.05953,-0.716109245731215));
#4558=CARTESIAN_POINT('Ctrl Pts',(-0.803348093619616,-0.05953,-0.716109245731215));
#4559=CARTESIAN_POINT('Ctrl Pts',(-0.807662468433795,-0.0925528133349865,
-0.711269279199862));
#4560=CARTESIAN_POINT('Ctrl Pts',(-0.815669690204649,-0.124911173756694,
-0.702247233627224));
#4561=CARTESIAN_POINT('Ctrl Pts',(-0.835214876415962,-0.177924977804098,
-0.678808213394124));
#4562=CARTESIAN_POINT('Ctrl Pts',(-0.845715984518854,-0.199697230012983,
-0.66581473268113));
#4563=CARTESIAN_POINT('Ctrl Pts',(-0.868789784891799,-0.237895043532788,
-0.635412538795143));
#4564=CARTESIAN_POINT('Ctrl Pts',(-0.8813524085237,-0.254319232363049,-0.617994461173994));
#4565=CARTESIAN_POINT('Ctrl Pts',(-0.906170138993533,-0.28018331644634,
-0.580957796077826));
#4566=CARTESIAN_POINT('Ctrl Pts',(-0.91968254693063,-0.29104845371857,-0.559515758398093));
#4567=CARTESIAN_POINT('Ctrl Pts',(-0.945943877838127,-0.30527573347708,
-0.51387163140139));
#4568=CARTESIAN_POINT('Ctrl Pts',(-0.958671816228589,-0.308638795020976,
-0.489657758261848));
#4569=CARTESIAN_POINT('Ctrl Pts',(-0.980551951791748,-0.308638795020976,
-0.444223188605045));
#4570=CARTESIAN_POINT('Ctrl Pts',(-0.99154738033959,-0.30527573347708,-0.419174982698463));
#4571=CARTESIAN_POINT('Ctrl Pts',(-1.01085972381132,-0.29104845371857,-0.370184399726282));
#4572=CARTESIAN_POINT('Ctrl Pts',(-1.01919893537026,-0.28018331644634,-0.346251081972725));
#4573=CARTESIAN_POINT('Ctrl Pts',(-1.03268176429485,-0.254319232363049,
-0.303755815985685));
#4574=CARTESIAN_POINT('Ctrl Pts',(-1.03846709802406,-0.237895043532788,
-0.283073967563097));
#4575=CARTESIAN_POINT('Ctrl Pts',(-1.04785021111757,-0.199697230012983,
-0.246078686169302));
#4576=CARTESIAN_POINT('Ctrl Pts',(-1.05146158959546,-0.177924977804098,
-0.229767286538461));
#4577=CARTESIAN_POINT('Ctrl Pts',(-1.05760072925372,-0.124911173756694,
-0.199872254546858));
#4578=CARTESIAN_POINT('Ctrl Pts',(-1.05966202740332,-0.0925528133349864,
-0.187986803072857));
#4579=CARTESIAN_POINT('Ctrl Pts',(-1.06075609691358,-0.05953,-0.181596019242328));
#4580=CARTESIAN_POINT('Origin',(-0.991065754692661,-0.05953,-0.477272113029314));
#4581=CARTESIAN_POINT('Origin',(0.,-0.05953,0.));
#4582=CARTESIAN_POINT('',(-0.519393123750572,-0.05953,-0.942555777842682));
#4583=CARTESIAN_POINT('Origin',(0.,-0.05953,0.));
#4584=CARTESIAN_POINT('Origin',(-0.244773027351946,-0.05953,-1.07242070340001));
#4585=CARTESIAN_POINT('Origin',(-0.244773027351946,0.,-1.07242070340001));
#4586=CARTESIAN_POINT('',(0.0589974094846125,-0.05953,-1.07456964270265));
#4587=CARTESIAN_POINT('Ctrl Pts',(0.0589974094846127,-0.05953,-1.07456964270265));
#4588=CARTESIAN_POINT('Ctrl Pts',(0.0525234025782722,-0.0925528133349865,
-1.07492508698591));
#4589=CARTESIAN_POINT('Ctrl Pts',(0.0404772621979744,-0.124911173756694,
-1.07556023164702));
#4590=CARTESIAN_POINT('Ctrl Pts',(0.0099656739833481,-0.177924977804098,
-1.07622728347683));
#4591=CARTESIAN_POINT('Ctrl Pts',(-0.00674037211528096,-0.199697230012983,
-1.07633607767727));
#4592=CARTESIAN_POINT('Ctrl Pts',(-0.044896043654098,-0.237895043532788,
-1.07542044338697));
#4593=CARTESIAN_POINT('Ctrl Pts',(-0.0663467128214644,-0.254319232363049,
-1.07438230428002));
#4594=CARTESIAN_POINT('Ctrl Pts',(-0.110776745452493,-0.28018331644634,
-1.07069360430242));
#4595=CARTESIAN_POINT('Ctrl Pts',(-0.135965654106109,-0.29104845371857,
-1.06788913840721));
#4596=CARTESIAN_POINT('Ctrl Pts',(-0.188025341585962,-0.30527573347708,
-1.05996242598502));
#4597=CARTESIAN_POINT('Ctrl Pts',(-0.214892249704082,-0.308638795020976,
-1.05481642595959));
#4598=CARTESIAN_POINT('Ctrl Pts',(-0.264056468041074,-0.308638795020976,
-1.04359501395068));
#4599=CARTESIAN_POINT('Ctrl Pts',(-0.290495481564827,-0.30527573347708,
-1.036574285215));
#4600=CARTESIAN_POINT('Ctrl Pts',(-0.340838910881557,-0.291048453718569,
-1.02112815447116));
#4601=CARTESIAN_POINT('Ctrl Pts',(-0.364750145543744,-0.28018331644634,
-1.01272583306292));
#4602=CARTESIAN_POINT('Ctrl Pts',(-0.406380688682952,-0.254319232363049,
-0.996771768218699));
#4603=CARTESIAN_POINT('Ctrl Pts',(-0.426157505475872,-0.237895043532788,
-0.988400002689705));
#4604=CARTESIAN_POINT('Ctrl Pts',(-0.460931856495794,-0.199697230012983,
-0.972669835243841));
#4605=CARTESIAN_POINT('Ctrl Pts',(-0.475936279901919,-0.177924977804098,
-0.965323333309091));
#4606=CARTESIAN_POINT('Ctrl Pts',(-0.503136848051454,-0.124911173756694,
-0.951483858396181));
#4607=CARTESIAN_POINT('Ctrl Pts',(-0.513714466572041,-0.0925528133349865,
-0.945684988399766));
#4608=CARTESIAN_POINT('Ctrl Pts',(-0.519393123750572,-0.05953,-0.942555777842682));
#4609=CARTESIAN_POINT('Origin',(-0.244773027351946,-0.05953,-1.07242070340001));
#4610=CARTESIAN_POINT('Origin',(0.,-0.05953,0.));
#4611=CARTESIAN_POINT('',(0.413083465285518,-0.05953,-0.993751811093549));
#4612=CARTESIAN_POINT('Origin',(0.,-0.05953,0.));
#4613=CARTESIAN_POINT('Origin',(0.685838782044607,-0.05953,-0.860014630714833));
#4614=CARTESIAN_POINT('Origin',(0.685838782044607,0.,-0.860014630714833));
#4615=CARTESIAN_POINT('',(0.876916659919095,-0.05953,-0.623857181492959));
#4616=CARTESIAN_POINT('Ctrl Pts',(0.876916659919095,-0.05953,-0.623857181492958));
#4617=CARTESIAN_POINT('Ctrl Pts',(0.873158080166742,-0.0925528133349865,
-0.62914037979579));
#4618=CARTESIAN_POINT('Ctrl Pts',(0.866144010579847,-0.124911173756694,
-0.638954437806245));
#4619=CARTESIAN_POINT('Ctrl Pts',(0.847641868610495,-0.177924977804098,
-0.663225258065736));
#4620=CARTESIAN_POINT('Ctrl Pts',(0.837310877969633,-0.199697230012983,
-0.676354402927683));
#4621=CARTESIAN_POINT('Ctrl Pts',(0.81280533416753,-0.237895043532788,-0.705614819529209));
#4622=CARTESIAN_POINT('Ctrl Pts',(0.798619410861634,-0.254319232363049,
-0.721738358858166));
#4623=CARTESIAN_POINT('Ctrl Pts',(0.768033796848072,-0.28018331644634,-0.754175290318038));
#4624=CARTESIAN_POINT('Ctrl Pts',(0.750136149454208,-0.29104845371857,-0.772120216227122));
#4625=CARTESIAN_POINT('Ctrl Pts',(0.711480111898423,-0.30527573347708,-0.807879894508811));
#4626=CARTESIAN_POINT('Ctrl Pts',(0.690705563850638,-0.308638795020976,
-0.825676810575913));
#4627=CARTESIAN_POINT('Ctrl Pts',(0.651278921914856,-0.308638795020976,
-0.857118508332695));
#4628=CARTESIAN_POINT('Ctrl Pts',(0.629305439856167,-0.30527573347708,-0.873412008702649));
#4629=CARTESIAN_POINT('Ctrl Pts',(0.585840553788742,-0.29104845371857,-0.903141581680914));
#4630=CARTESIAN_POINT('Ctrl Pts',(0.564362943424239,-0.28018331644634,-0.916597376014514));
#4631=CARTESIAN_POINT('Ctrl Pts',(0.525933334162556,-0.254319232363049,
-0.939198248544427));
#4632=CARTESIAN_POINT('Ctrl Pts',(0.507057380724533,-0.237895043532788,
-0.949440676105255));
#4633=CARTESIAN_POINT('Ctrl Pts',(0.473077587363686,-0.199697230012983,
-0.966820759530997));
#4634=CARTESIAN_POINT('Ctrl Pts',(0.457978755888596,-0.177924977804098,
-0.973971221090534));
#4635=CARTESIAN_POINT('Ctrl Pts',(0.430199341854858,-0.124911173756694,
-0.986608710139579));
#4636=CARTESIAN_POINT('Ctrl Pts',(0.419070565453384,-0.0925528133349865,
-0.991263089003441));
#4637=CARTESIAN_POINT('Ctrl Pts',(0.413083465285518,-0.05953,-0.993751811093549));
#4638=CARTESIAN_POINT('Origin',(0.685838782044607,-0.05953,-0.860014630714833));
#4639=CARTESIAN_POINT('Origin',(0.,-0.208355,0.));
#4640=CARTESIAN_POINT('',(-1.076188,-0.35718,1.31795018948079E-16));
#4641=CARTESIAN_POINT('Origin',(0.,-0.35718,0.));
#4642=CARTESIAN_POINT('',(-1.076188,-0.208355,1.31795018948079E-16));
#4643=CARTESIAN_POINT('',(1.03449977959455,-0.05953,0.296632461748266));
#4644=CARTESIAN_POINT('Origin',(0.,-0.05953,0.));
#4645=CARTESIAN_POINT('',(1.03449977959455,-0.05953,-0.296632461748266));
#4646=CARTESIAN_POINT('Ctrl Pts',(1.03449977959455,-0.05953,0.296632461748267));
#4647=CARTESIAN_POINT('Ctrl Pts',(1.03628691421076,-0.0925528133349865,
0.290399865505497));
#4648=CARTESIAN_POINT('Ctrl Pts',(1.03958665287714,-0.124911173756694,0.278797079997872));
#4649=CARTESIAN_POINT('Ctrl Pts',(1.0470264474309,-0.177924977804098,0.249198913998601));
#4650=CARTESIAN_POINT('Ctrl Pts',(1.05084995891418,-0.199697230012983,0.232935932341942));
#4651=CARTESIAN_POINT('Ctrl Pts',(1.05844771715377,-0.237895043532788,0.195533155353269));
#4652=CARTESIAN_POINT('Ctrl Pts',(1.06220882929878,-0.254319232363049,0.17438929156337));
#4653=CARTESIAN_POINT('Ctrl Pts',(1.06849922508772,-0.28018331644634,0.130252399648131));
#4654=CARTESIAN_POINT('Ctrl Pts',(1.07137013248666,-0.29104845371857,0.105070977154072));
#4655=CARTESIAN_POINT('Ctrl Pts',(1.07522652957392,-0.30527573347708,0.0525526752791107));
#4656=CARTESIAN_POINT('Ctrl Pts',(1.076188,-0.308638795020976,0.025214283908933));
#4657=CARTESIAN_POINT('Ctrl Pts',(1.076188,-0.308638795020976,-0.025214283908933));
#4658=CARTESIAN_POINT('Ctrl Pts',(1.07522652957392,-0.30527573347708,-0.0525526752791107));
#4659=CARTESIAN_POINT('Ctrl Pts',(1.07137013248666,-0.29104845371857,-0.105070977154072));
#4660=CARTESIAN_POINT('Ctrl Pts',(1.06849922508772,-0.28018331644634,-0.130252399648131));
#4661=CARTESIAN_POINT('Ctrl Pts',(1.06220882929878,-0.254319232363049,-0.17438929156337));
#4662=CARTESIAN_POINT('Ctrl Pts',(1.05844771715377,-0.237895043532788,-0.195533155353269));
#4663=CARTESIAN_POINT('Ctrl Pts',(1.05084995891418,-0.199697230012983,-0.232935932341942));
#4664=CARTESIAN_POINT('Ctrl Pts',(1.0470264474309,-0.177924977804098,-0.249198913998601));
#4665=CARTESIAN_POINT('Ctrl Pts',(1.03958665287714,-0.124911173756694,-0.278797079997872));
#4666=CARTESIAN_POINT('Ctrl Pts',(1.03628691421076,-0.0925528133349865,
-0.290399865505497));
#4667=CARTESIAN_POINT('Ctrl Pts',(1.03449977959455,-0.05953,-0.296632461748267));
#4668=CARTESIAN_POINT('Origin',(0.,-0.05953,0.));
#4669=CARTESIAN_POINT('Origin',(0.,-0.05953,0.));
#4670=CARTESIAN_POINT('Origin',(1.1,-0.05953,0.));
#4671=CARTESIAN_POINT('Origin',(1.1,0.,0.));
#4672=CARTESIAN_POINT('Origin',(1.1,-0.05953,0.));
#4673=CARTESIAN_POINT('Origin',(0.,-0.35718,0.));
#4674=CARTESIAN_POINT('Origin',(0.,-0.05953,0.));
#4675=CARTESIAN_POINT('',(0.,0.,0.));
#4676=CARTESIAN_POINT('Origin',(1.119765,0.495,0.));
#4677=CARTESIAN_POINT('',(-1.119765,0.495,-1.37131662304724E-16));
#4678=CARTESIAN_POINT('Origin',(0.,0.495,0.));
#4679=CARTESIAN_POINT('',(-1.085235,0.495,-1.32902956907268E-16));
#4680=CARTESIAN_POINT('Origin',(0.,0.495,0.));
#4681=CARTESIAN_POINT('Origin',(0.,0.4575,0.));
#4682=CARTESIAN_POINT('',(-1.119765,0.42,-1.37131662304724E-16));
#4683=CARTESIAN_POINT('Origin',(0.,0.42,0.));
#4684=CARTESIAN_POINT('',(-1.119765,0.4575,-1.37131662304724E-16));
#4685=CARTESIAN_POINT('Origin',(1.085235,0.42,0.));
#4686=CARTESIAN_POINT('',(-1.085235,0.42,-1.32902956907268E-16));
#4687=CARTESIAN_POINT('Origin',(0.,0.42,0.));
#4688=CARTESIAN_POINT('Origin',(0.,0.4575,0.));
#4689=CARTESIAN_POINT('',(-1.085235,0.4575,-1.32902956907268E-16));
#4690=CARTESIAN_POINT('Origin',(1.119765,-0.42,0.));
#4691=CARTESIAN_POINT('',(-1.119765,-0.42,-1.37131662304724E-16));
#4692=CARTESIAN_POINT('Origin',(0.,-0.42,0.));
#4693=CARTESIAN_POINT('',(-1.085235,-0.42,-1.32902956907268E-16));
#4694=CARTESIAN_POINT('Origin',(0.,-0.42,0.));
#4695=CARTESIAN_POINT('Origin',(0.,-0.4575,0.));
#4696=CARTESIAN_POINT('',(-1.119765,-0.495,-1.37131662304724E-16));
#4697=CARTESIAN_POINT('Origin',(0.,-0.495,0.));
#4698=CARTESIAN_POINT('',(-1.119765,-0.4575,-1.37131662304724E-16));
#4699=CARTESIAN_POINT('Origin',(1.085235,-0.495,0.));
#4700=CARTESIAN_POINT('',(-1.085235,-0.495,-1.32902956907268E-16));
#4701=CARTESIAN_POINT('Origin',(0.,-0.495,0.));
#4702=CARTESIAN_POINT('Origin',(0.,-0.4575,0.));
#4703=CARTESIAN_POINT('',(-1.085235,-0.4575,-1.32902956907268E-16));
#4704=CARTESIAN_POINT('',(0.,0.,0.));
#4705=CARTESIAN_POINT('',(0.,0.,0.));
#4706=CARTESIAN_POINT('',(0.,0.,0.));
#4707=CARTESIAN_POINT('',(0.,0.,0.));
#4708=CARTESIAN_POINT('',(0.,0.,0.));
#4709=CARTESIAN_POINT('',(0.,0.,0.));
#4710=CARTESIAN_POINT('Origin',(0.,1.1,3.5));
#4711=CARTESIAN_POINT('',(-1.2,1.3,3.5));
#4712=CARTESIAN_POINT('Origin',(0.,1.3,3.5));
#4713=CARTESIAN_POINT('',(-1.2,1.1,3.5));
#4714=CARTESIAN_POINT('',(-1.2,1.1,3.5));
#4715=CARTESIAN_POINT('Origin',(0.,1.1,3.5));
#4716=CARTESIAN_POINT('Origin',(0.,1.1,3.5));
#4717=CARTESIAN_POINT('',(-1.6,1.3,3.5));
#4718=CARTESIAN_POINT('Origin',(0.,1.3,3.5));
#4719=CARTESIAN_POINT('',(-1.6,1.1,3.5));
#4720=CARTESIAN_POINT('',(-1.6,1.1,3.5));
#4721=CARTESIAN_POINT('Origin',(0.,1.1,3.5));
#4722=CARTESIAN_POINT('Origin',(0.,1.3,3.5));
#4723=CARTESIAN_POINT('Origin',(0.,1.1,3.5));
#4724=CARTESIAN_POINT('',(-5.,3.,9.75));
#4725=CARTESIAN_POINT('',(-5.,2.4,13.75));
#4726=CARTESIAN_POINT('',(-5.,3.6,13.75));
#4727=CARTESIAN_POINT('',(-5.,3.,10.25));
#4728=CARTESIAN_POINT('',(-5.,0.6,10.25));
#4729=CARTESIAN_POINT('',(0.,0.,0.));
#4730=CARTESIAN_POINT('',(0.,0.,0.));
#4731=CARTESIAN_POINT('',(10.7850124367643,-2.43138842392909E-14,0.311394004343978));
#4732=CARTESIAN_POINT('',(10.6296948476887,-6.,0.245591981804335));
#4733=CARTESIAN_POINT('',(-0.325640445426777,-5.99999999999998,-0.114085355859928));
#4734=UNCERTAINTY_MEASURE_WITH_UNIT(LENGTH_MEASURE(0.001),#4778,
'DISTANCE_ACCURACY_VALUE',
'Maximum model space distance between geometric entities at asserted c
onnectivities');
#4735=UNCERTAINTY_MEASURE_WITH_UNIT(LENGTH_MEASURE(0.001),#4778,
'DISTANCE_ACCURACY_VALUE',
'Maximum model space distance between geometric entities at asserted c
onnectivities');
#4736=UNCERTAINTY_MEASURE_WITH_UNIT(LENGTH_MEASURE(0.001),#4778,
'DISTANCE_ACCURACY_VALUE',
'Maximum model space distance between geometric entities at asserted c
onnectivities');
#4737=UNCERTAINTY_MEASURE_WITH_UNIT(LENGTH_MEASURE(0.001),#4778,
'DISTANCE_ACCURACY_VALUE',
'Maximum model space distance between geometric entities at asserted c
onnectivities');
#4738=UNCERTAINTY_MEASURE_WITH_UNIT(LENGTH_MEASURE(0.001),#4778,
'DISTANCE_ACCURACY_VALUE',
'Maximum model space distance between geometric entities at asserted c
onnectivities');
#4739=UNCERTAINTY_MEASURE_WITH_UNIT(LENGTH_MEASURE(0.001),#4778,
'DISTANCE_ACCURACY_VALUE',
'Maximum model space distance between geometric entities at asserted c
onnectivities');
#4740=UNCERTAINTY_MEASURE_WITH_UNIT(LENGTH_MEASURE(0.001),#4778,
'DISTANCE_ACCURACY_VALUE',
'Maximum model space distance between geometric entities at asserted c
onnectivities');
#4741=UNCERTAINTY_MEASURE_WITH_UNIT(LENGTH_MEASURE(0.001),#4778,
'DISTANCE_ACCURACY_VALUE',
'Maximum model space distance between geometric entities at asserted c
onnectivities');
#4742=UNCERTAINTY_MEASURE_WITH_UNIT(LENGTH_MEASURE(0.001),#4778,
'DISTANCE_ACCURACY_VALUE',
'Maximum model space distance between geometric entities at asserted c
onnectivities');
#4743=UNCERTAINTY_MEASURE_WITH_UNIT(LENGTH_MEASURE(0.001),#4778,
'DISTANCE_ACCURACY_VALUE',
'Maximum model space distance between geometric entities at asserted c
onnectivities');
#4744=UNCERTAINTY_MEASURE_WITH_UNIT(LENGTH_MEASURE(0.001),#4778,
'DISTANCE_ACCURACY_VALUE',
'Maximum model space distance between geometric entities at asserted c
onnectivities');
#4745=UNCERTAINTY_MEASURE_WITH_UNIT(LENGTH_MEASURE(0.001),#4778,
'DISTANCE_ACCURACY_VALUE',
'Maximum model space distance between geometric entities at asserted c
onnectivities');
#4746=UNCERTAINTY_MEASURE_WITH_UNIT(LENGTH_MEASURE(0.001),#4778,
'DISTANCE_ACCURACY_VALUE',
'Maximum model space distance between geometric entities at asserted c
onnectivities');
#4747=UNCERTAINTY_MEASURE_WITH_UNIT(LENGTH_MEASURE(0.001),#4778,
'DISTANCE_ACCURACY_VALUE',
'Maximum model space distance between geometric entities at asserted c
onnectivities');
#4748=UNCERTAINTY_MEASURE_WITH_UNIT(LENGTH_MEASURE(0.001),#4778,
'DISTANCE_ACCURACY_VALUE',
'Maximum model space distance between geometric entities at asserted c
onnectivities');
#4749=UNCERTAINTY_MEASURE_WITH_UNIT(LENGTH_MEASURE(0.001),#4778,
'DISTANCE_ACCURACY_VALUE',
'Maximum model space distance between geometric entities at asserted c
onnectivities');
#4750=UNCERTAINTY_MEASURE_WITH_UNIT(LENGTH_MEASURE(0.001),#4778,
'DISTANCE_ACCURACY_VALUE',
'Maximum model space distance between geometric entities at asserted c
onnectivities');
#4751=UNCERTAINTY_MEASURE_WITH_UNIT(LENGTH_MEASURE(0.001),#4778,
'DISTANCE_ACCURACY_VALUE',
'Maximum model space distance between geometric entities at asserted c
onnectivities');
#4752=UNCERTAINTY_MEASURE_WITH_UNIT(LENGTH_MEASURE(0.001),#4778,
'DISTANCE_ACCURACY_VALUE',
'Maximum model space distance between geometric entities at asserted c
onnectivities');
#4753=UNCERTAINTY_MEASURE_WITH_UNIT(LENGTH_MEASURE(0.001),#4778,
'DISTANCE_ACCURACY_VALUE',
'Maximum model space distance between geometric entities at asserted c
onnectivities');
#4754=UNCERTAINTY_MEASURE_WITH_UNIT(LENGTH_MEASURE(0.001),#4778,
'DISTANCE_ACCURACY_VALUE',
'Maximum model space distance between geometric entities at asserted c
onnectivities');
#4755=UNCERTAINTY_MEASURE_WITH_UNIT(LENGTH_MEASURE(0.001),#4778,
'DISTANCE_ACCURACY_VALUE',
'Maximum model space distance between geometric entities at asserted c
onnectivities');
#4756=(
GEOMETRIC_REPRESENTATION_CONTEXT(3)
GLOBAL_UNCERTAINTY_ASSIGNED_CONTEXT((#4734))
GLOBAL_UNIT_ASSIGNED_CONTEXT((#4778,#4780,#4781))
REPRESENTATION_CONTEXT('','3D')
);
#4757=(
GEOMETRIC_REPRESENTATION_CONTEXT(3)
GLOBAL_UNCERTAINTY_ASSIGNED_CONTEXT((#4735))
GLOBAL_UNIT_ASSIGNED_CONTEXT((#4778,#4780,#4781))
REPRESENTATION_CONTEXT('','3D')
);
#4758=(
GEOMETRIC_REPRESENTATION_CONTEXT(3)
GLOBAL_UNCERTAINTY_ASSIGNED_CONTEXT((#4736))
GLOBAL_UNIT_ASSIGNED_CONTEXT((#4778,#4780,#4781))
REPRESENTATION_CONTEXT('','3D')
);
#4759=(
GEOMETRIC_REPRESENTATION_CONTEXT(3)
GLOBAL_UNCERTAINTY_ASSIGNED_CONTEXT((#4737))
GLOBAL_UNIT_ASSIGNED_CONTEXT((#4778,#4780,#4781))
REPRESENTATION_CONTEXT('','3D')
);
#4760=(
GEOMETRIC_REPRESENTATION_CONTEXT(3)
GLOBAL_UNCERTAINTY_ASSIGNED_CONTEXT((#4738))
GLOBAL_UNIT_ASSIGNED_CONTEXT((#4778,#4780,#4781))
REPRESENTATION_CONTEXT('','3D')
);
#4761=(
GEOMETRIC_REPRESENTATION_CONTEXT(3)
GLOBAL_UNCERTAINTY_ASSIGNED_CONTEXT((#4739))
GLOBAL_UNIT_ASSIGNED_CONTEXT((#4778,#4780,#4781))
REPRESENTATION_CONTEXT('','3D')
);
#4762=(
GEOMETRIC_REPRESENTATION_CONTEXT(3)
GLOBAL_UNCERTAINTY_ASSIGNED_CONTEXT((#4740))
GLOBAL_UNIT_ASSIGNED_CONTEXT((#4778,#4780,#4781))
REPRESENTATION_CONTEXT('','3D')
);
#4763=(
GEOMETRIC_REPRESENTATION_CONTEXT(3)
GLOBAL_UNCERTAINTY_ASSIGNED_CONTEXT((#4741))
GLOBAL_UNIT_ASSIGNED_CONTEXT((#4778,#4780,#4781))
REPRESENTATION_CONTEXT('','3D')
);
#4764=(
GEOMETRIC_REPRESENTATION_CONTEXT(3)
GLOBAL_UNCERTAINTY_ASSIGNED_CONTEXT((#4742))
GLOBAL_UNIT_ASSIGNED_CONTEXT((#4778,#4780,#4781))
REPRESENTATION_CONTEXT('','3D')
);
#4765=(
GEOMETRIC_REPRESENTATION_CONTEXT(3)
GLOBAL_UNCERTAINTY_ASSIGNED_CONTEXT((#4743))
GLOBAL_UNIT_ASSIGNED_CONTEXT((#4778,#4780,#4781))
REPRESENTATION_CONTEXT('','3D')
);
#4766=(
GEOMETRIC_REPRESENTATION_CONTEXT(3)
GLOBAL_UNCERTAINTY_ASSIGNED_CONTEXT((#4744))
GLOBAL_UNIT_ASSIGNED_CONTEXT((#4778,#4780,#4781))
REPRESENTATION_CONTEXT('','3D')
);
#4767=(
GEOMETRIC_REPRESENTATION_CONTEXT(3)
GLOBAL_UNCERTAINTY_ASSIGNED_CONTEXT((#4745))
GLOBAL_UNIT_ASSIGNED_CONTEXT((#4778,#4780,#4781))
REPRESENTATION_CONTEXT('','3D')
);
#4768=(
GEOMETRIC_REPRESENTATION_CONTEXT(3)
GLOBAL_UNCERTAINTY_ASSIGNED_CONTEXT((#4746))
GLOBAL_UNIT_ASSIGNED_CONTEXT((#4778,#4780,#4781))
REPRESENTATION_CONTEXT('','3D')
);
#4769=(
GEOMETRIC_REPRESENTATION_CONTEXT(3)
GLOBAL_UNCERTAINTY_ASSIGNED_CONTEXT((#4747))
GLOBAL_UNIT_ASSIGNED_CONTEXT((#4778,#4780,#4781))
REPRESENTATION_CONTEXT('','3D')
);
#4770=(
GEOMETRIC_REPRESENTATION_CONTEXT(3)
GLOBAL_UNCERTAINTY_ASSIGNED_CONTEXT((#4748))
GLOBAL_UNIT_ASSIGNED_CONTEXT((#4778,#4780,#4781))
REPRESENTATION_CONTEXT('','3D')
);
#4771=(
GEOMETRIC_REPRESENTATION_CONTEXT(3)
GLOBAL_UNCERTAINTY_ASSIGNED_CONTEXT((#4749))
GLOBAL_UNIT_ASSIGNED_CONTEXT((#4778,#4780,#4781))
REPRESENTATION_CONTEXT('','3D')
);
#4772=(
GEOMETRIC_REPRESENTATION_CONTEXT(3)
GLOBAL_UNCERTAINTY_ASSIGNED_CONTEXT((#4750))
GLOBAL_UNIT_ASSIGNED_CONTEXT((#4778,#4780,#4781))
REPRESENTATION_CONTEXT('','3D')
);
#4773=(
GEOMETRIC_REPRESENTATION_CONTEXT(3)
GLOBAL_UNCERTAINTY_ASSIGNED_CONTEXT((#4751))
GLOBAL_UNIT_ASSIGNED_CONTEXT((#4778,#4780,#4781))
REPRESENTATION_CONTEXT('','3D')
);
#4774=(
GEOMETRIC_REPRESENTATION_CONTEXT(3)
GLOBAL_UNCERTAINTY_ASSIGNED_CONTEXT((#4752))
GLOBAL_UNIT_ASSIGNED_CONTEXT((#4778,#4780,#4781))
REPRESENTATION_CONTEXT('','3D')
);
#4775=(
GEOMETRIC_REPRESENTATION_CONTEXT(3)
GLOBAL_UNCERTAINTY_ASSIGNED_CONTEXT((#4753))
GLOBAL_UNIT_ASSIGNED_CONTEXT((#4778,#4780,#4781))
REPRESENTATION_CONTEXT('','3D')
);
#4776=(
GEOMETRIC_REPRESENTATION_CONTEXT(3)
GLOBAL_UNCERTAINTY_ASSIGNED_CONTEXT((#4754))
GLOBAL_UNIT_ASSIGNED_CONTEXT((#4778,#4780,#4781))
REPRESENTATION_CONTEXT('','3D')
);
#4777=(
GEOMETRIC_REPRESENTATION_CONTEXT(3)
GLOBAL_UNCERTAINTY_ASSIGNED_CONTEXT((#4755))
GLOBAL_UNIT_ASSIGNED_CONTEXT((#4778,#4780,#4781))
REPRESENTATION_CONTEXT('','3D')
);
#4778=(
LENGTH_UNIT()
NAMED_UNIT(*)
SI_UNIT(.CENTI.,.METRE.)
);
#4779=(
LENGTH_UNIT()
NAMED_UNIT(*)
SI_UNIT($,.METRE.)
);
#4780=(
NAMED_UNIT(*)
PLANE_ANGLE_UNIT()
SI_UNIT($,.RADIAN.)
);
#4781=(
NAMED_UNIT(*)
SI_UNIT($,.STERADIAN.)
SOLID_ANGLE_UNIT()
);
#4782=SHAPE_DEFINITION_REPRESENTATION(#4803,#4871);
#4783=SHAPE_DEFINITION_REPRESENTATION(#4804,#4872);
#4784=SHAPE_DEFINITION_REPRESENTATION(#4805,#4873);
#4785=SHAPE_DEFINITION_REPRESENTATION(#4806,#4874);
#4786=SHAPE_DEFINITION_REPRESENTATION(#4807,#4875);
#4787=SHAPE_DEFINITION_REPRESENTATION(#4808,#4876);
#4788=SHAPE_DEFINITION_REPRESENTATION(#4809,#4877);
#4789=SHAPE_DEFINITION_REPRESENTATION(#4810,#4878);
#4790=SHAPE_DEFINITION_REPRESENTATION(#4811,#4879);
#4791=SHAPE_DEFINITION_REPRESENTATION(#4812,#4880);
#4792=SHAPE_DEFINITION_REPRESENTATION(#4813,#4881);
#4793=SHAPE_DEFINITION_REPRESENTATION(#4814,#4882);
#4794=SHAPE_DEFINITION_REPRESENTATION(#4847,#4883);
#4795=SHAPE_DEFINITION_REPRESENTATION(#4848,#4884);
#4796=SHAPE_DEFINITION_REPRESENTATION(#4849,#4885);
#4797=SHAPE_DEFINITION_REPRESENTATION(#4850,#4886);
#4798=SHAPE_DEFINITION_REPRESENTATION(#4851,#4887);
#4799=SHAPE_DEFINITION_REPRESENTATION(#4852,#4888);
#4800=SHAPE_DEFINITION_REPRESENTATION(#4853,#4889);
#4801=SHAPE_DEFINITION_REPRESENTATION(#4854,#4890);
#4802=SHAPE_DEFINITION_REPRESENTATION(#4860,#4891);
#4803=PRODUCT_DEFINITION_SHAPE('',$,#4893);
#4804=PRODUCT_DEFINITION_SHAPE('',$,#4894);
#4805=PRODUCT_DEFINITION_SHAPE('',$,#4895);
#4806=PRODUCT_DEFINITION_SHAPE('',$,#4896);
#4807=PRODUCT_DEFINITION_SHAPE('',$,#4897);
#4808=PRODUCT_DEFINITION_SHAPE('',$,#4898);
#4809=PRODUCT_DEFINITION_SHAPE('',$,#4899);
#4810=PRODUCT_DEFINITION_SHAPE('',$,#4900);
#4811=PRODUCT_DEFINITION_SHAPE('',$,#4901);
#4812=PRODUCT_DEFINITION_SHAPE('',$,#4902);
#4813=PRODUCT_DEFINITION_SHAPE('',$,#4903);
#4814=PRODUCT_DEFINITION_SHAPE('',$,#4904);
#4815=PRODUCT_DEFINITION_SHAPE($,$,#182);
#4816=PRODUCT_DEFINITION_SHAPE($,$,#183);
#4817=PRODUCT_DEFINITION_SHAPE($,$,#184);
#4818=PRODUCT_DEFINITION_SHAPE($,$,#185);
#4819=PRODUCT_DEFINITION_SHAPE($,$,#186);
#4820=PRODUCT_DEFINITION_SHAPE($,$,#187);
#4821=PRODUCT_DEFINITION_SHAPE($,$,#188);
#4822=PRODUCT_DEFINITION_SHAPE($,$,#189);
#4823=PRODUCT_DEFINITION_SHAPE($,$,#190);
#4824=PRODUCT_DEFINITION_SHAPE($,$,#191);
#4825=PRODUCT_DEFINITION_SHAPE($,$,#192);
#4826=PRODUCT_DEFINITION_SHAPE($,$,#193);
#4827=PRODUCT_DEFINITION_SHAPE($,$,#194);
#4828=PRODUCT_DEFINITION_SHAPE($,$,#195);
#4829=PRODUCT_DEFINITION_SHAPE($,$,#196);
#4830=PRODUCT_DEFINITION_SHAPE($,$,#197);
#4831=PRODUCT_DEFINITION_SHAPE($,$,#198);
#4832=PRODUCT_DEFINITION_SHAPE($,$,#199);
#4833=PRODUCT_DEFINITION_SHAPE($,$,#200);
#4834=PRODUCT_DEFINITION_SHAPE($,$,#201);
#4835=PRODUCT_DEFINITION_SHAPE($,$,#202);
#4836=PRODUCT_DEFINITION_SHAPE($,$,#203);
#4837=PRODUCT_DEFINITION_SHAPE($,$,#204);
#4838=PRODUCT_DEFINITION_SHAPE($,$,#205);
#4839=PRODUCT_DEFINITION_SHAPE($,$,#206);
#4840=PRODUCT_DEFINITION_SHAPE($,$,#207);
#4841=PRODUCT_DEFINITION_SHAPE($,$,#208);
#4842=PRODUCT_DEFINITION_SHAPE($,$,#209);
#4843=PRODUCT_DEFINITION_SHAPE($,$,#210);
#4844=PRODUCT_DEFINITION_SHAPE($,$,#211);
#4845=PRODUCT_DEFINITION_SHAPE($,$,#212);
#4846=PRODUCT_DEFINITION_SHAPE($,$,#213);
#4847=PRODUCT_DEFINITION_SHAPE('',$,#4905);
#4848=PRODUCT_DEFINITION_SHAPE('',$,#4906);
#4849=PRODUCT_DEFINITION_SHAPE('',$,#4907);
#4850=PRODUCT_DEFINITION_SHAPE('',$,#4908);
#4851=PRODUCT_DEFINITION_SHAPE('',$,#4909);
#4852=PRODUCT_DEFINITION_SHAPE('',$,#4910);
#4853=PRODUCT_DEFINITION_SHAPE('',$,#4911);
#4854=PRODUCT_DEFINITION_SHAPE('',$,#4912);
#4855=PRODUCT_DEFINITION_SHAPE($,$,#214);
#4856=PRODUCT_DEFINITION_SHAPE($,$,#215);
#4857=PRODUCT_DEFINITION_SHAPE($,$,#216);
#4858=PRODUCT_DEFINITION_SHAPE($,$,#217);
#4859=PRODUCT_DEFINITION_SHAPE($,$,#218);
#4860=PRODUCT_DEFINITION_SHAPE('',$,#4913);
#4861=PRODUCT_DEFINITION_SHAPE($,$,#219);
#4862=PRODUCT_DEFINITION_SHAPE($,$,#220);
#4863=PRODUCT_DEFINITION_SHAPE($,$,#221);
#4864=PRODUCT_DEFINITION_SHAPE($,$,#222);
#4865=PRODUCT_DEFINITION_SHAPE($,$,#223);
#4866=PRODUCT_DEFINITION_SHAPE($,$,#224);
#4867=PRODUCT_DEFINITION_SHAPE($,$,#225);
#4868=PRODUCT_DEFINITION_SHAPE($,$,#226);
#4869=PRODUCT_DEFINITION_SHAPE($,$,#227);
#4870=PRODUCT_DEFINITION_SHAPE($,$,#228);
#4871=SHAPE_REPRESENTATION('',(#2579,#2927,#2928,#2929,#2930,#2931),#4756);
#4872=SHAPE_REPRESENTATION('',(#2580,#2735,#2736,#2737,#2738,#2739,#2740,
#2741,#2742,#2743,#2744,#2745,#2746,#2747,#2748,#2749,#2750,#2751,#2752,
#2753,#2754,#2755,#2756,#2757,#2758,#2759,#2760,#2761,#2762,#2763,#2764,
#2765,#2766),#4757);
#4873=SHAPE_REPRESENTATION('',(#2581),#4758);
#4874=SHAPE_REPRESENTATION('',(#2604),#4759);
#4875=SHAPE_REPRESENTATION('',(#2623),#4760);
#4876=SHAPE_REPRESENTATION('',(#2635),#4761);
#4877=SHAPE_REPRESENTATION('',(#2644),#4762);
#4878=SHAPE_REPRESENTATION('',(#2670),#4763);
#4879=SHAPE_REPRESENTATION('',(#2684),#4764);
#4880=SHAPE_REPRESENTATION('',(#2693),#4765);
#4881=SHAPE_REPRESENTATION('',(#2702),#4766);
#4882=SHAPE_REPRESENTATION('',(#2711),#4767);
#4883=SHAPE_REPRESENTATION('',(#2767,#2922,#2923,#2924,#2925,#2926),#4768);
#4884=SHAPE_REPRESENTATION('',(#2768),#4769);
#4885=SHAPE_REPRESENTATION('',(#2785,#2908,#2909,#2910,#2911,#2912),#4770);
#4886=SHAPE_REPRESENTATION('',(#2786),#4771);
#4887=SHAPE_REPRESENTATION('',(#2806),#4772);
#4888=SHAPE_REPRESENTATION('',(#2826),#4773);
#4889=SHAPE_REPRESENTATION('',(#2841),#4774);
#4890=SHAPE_REPRESENTATION('',(#2891),#4775);
#4891=SHAPE_REPRESENTATION('',(#2913),#4776);
#4892=PRODUCT_DEFINITION_CONTEXT('part definition',#4957,'design');
#4893=PRODUCT_DEFINITION('PAT-044',
'PAT-044',#4914,#4892);
#4894=PRODUCT_DEFINITION('Side frames axles and hanger',
'Side frames axles and hanger',#4915,#4892);
#4895=PRODUCT_DEFINITION('Lower cross member','Lower cross member',#4916,
#4892);
#4896=PRODUCT_DEFINITION('Side frame plate','Side frame plate',#4917,#4892);
#4897=PRODUCT_DEFINITION('Welded eye plate','Welded eye plate',#4918,#4892);
#4898=PRODUCT_DEFINITION('Flat Washer - M8','Flat Washer - M8',#4919,#4892);
#4899=PRODUCT_DEFINITION('Cap Screw - M8x30','Cap Screw - M8x30',#4920,
#4892);
#4900=PRODUCT_DEFINITION('Cantilever wheel axle',
'Cantilever wheel axle',#4921,#4892);
#4901=PRODUCT_DEFINITION('Inner bearing spacer','Inner bearing spacer',
#4922,#4892);
#4902=PRODUCT_DEFINITION('Outer bearing spacer','Outer bearing spacer',
#4923,#4892);
#4903=PRODUCT_DEFINITION('Axle keeper','Axle keeper',#4924,#4892);
#4904=PRODUCT_DEFINITION('M4x10 Cap Screw','M4x10 Cap Screw',#4925,#4892);
#4905=PRODUCT_DEFINITION('Wheel','Wheel',#4926,#4892);
#4906=PRODUCT_DEFINITION('Wheel with twelve millimetre bearings',
'Wheel with twelve millimetre bearings',#4927,#4892);
#4907=PRODUCT_DEFINITION('Sealed Ball Bearing - 12 x 32 x 10 mm',
'Sealed Ball Bearing - 12 x 32 x 10 mm',#4928,#4892);
#4908=PRODUCT_DEFINITION('Inner ring','Inner ring',#4929,#4892);
#4909=PRODUCT_DEFINITION('Outer ring','Outer ring',#4930,#4892);
#4910=PRODUCT_DEFINITION('Balls','Balls',#4931,#4892);
#4911=PRODUCT_DEFINITION('Cage','Cage',#4932,#4892);
#4912=PRODUCT_DEFINITION('Seals 2RS','Seals 2RS',#4933,#4892);
#4913=PRODUCT_DEFINITION('Bearing end retainer','Bearing end retainer',
#4934,#4892);
#4914=PRODUCT_DEFINITION_FORMATION('',$,#4959);
#4915=PRODUCT_DEFINITION_FORMATION('',$,#4960);
#4916=PRODUCT_DEFINITION_FORMATION('',$,#4961);
#4917=PRODUCT_DEFINITION_FORMATION('',$,#4962);
#4918=PRODUCT_DEFINITION_FORMATION('',$,#4963);
#4919=PRODUCT_DEFINITION_FORMATION('',$,#4964);
#4920=PRODUCT_DEFINITION_FORMATION('',$,#4965);
#4921=PRODUCT_DEFINITION_FORMATION('',$,#4966);
#4922=PRODUCT_DEFINITION_FORMATION('',$,#4967);
#4923=PRODUCT_DEFINITION_FORMATION('',$,#4968);
#4924=PRODUCT_DEFINITION_FORMATION('',$,#4969);
#4925=PRODUCT_DEFINITION_FORMATION('',$,#4970);
#4926=PRODUCT_DEFINITION_FORMATION('',$,#4971);
#4927=PRODUCT_DEFINITION_FORMATION('',$,#4972);
#4928=PRODUCT_DEFINITION_FORMATION('',$,#4973);
#4929=PRODUCT_DEFINITION_FORMATION('',$,#4974);
#4930=PRODUCT_DEFINITION_FORMATION('',$,#4975);
#4931=PRODUCT_DEFINITION_FORMATION('',$,#4976);
#4932=PRODUCT_DEFINITION_FORMATION('',$,#4977);
#4933=PRODUCT_DEFINITION_FORMATION('',$,#4978);
#4934=PRODUCT_DEFINITION_FORMATION('',$,#4979);
#4935=PRODUCT_RELATED_PRODUCT_CATEGORY('PAT-044',
'PAT-044',(#4959));
#4936=PRODUCT_RELATED_PRODUCT_CATEGORY('Side frames axles and hanger',
'Side frames axles and hanger',(#4960));
#4937=PRODUCT_RELATED_PRODUCT_CATEGORY('Lower cross member',
'Lower cross member',(#4961));
#4938=PRODUCT_RELATED_PRODUCT_CATEGORY('Side frame plate',
'Side frame plate',(#4962));
#4939=PRODUCT_RELATED_PRODUCT_CATEGORY('Welded eye plate',
'Welded eye plate',(#4963));
#4940=PRODUCT_RELATED_PRODUCT_CATEGORY('Flat Washer - M8',
'Flat Washer - M8',(#4964));
#4941=PRODUCT_RELATED_PRODUCT_CATEGORY('Cap Screw - M8x30',
'Cap Screw - M8x30',(#4965));
#4942=PRODUCT_RELATED_PRODUCT_CATEGORY('Cantilever wheel axle',
'Cantilever wheel axle',(#4966));
#4943=PRODUCT_RELATED_PRODUCT_CATEGORY('Inner bearing spacer',
'Inner bearing spacer',(#4967));
#4944=PRODUCT_RELATED_PRODUCT_CATEGORY('Outer bearing spacer',
'Outer bearing spacer',(#4968));
#4945=PRODUCT_RELATED_PRODUCT_CATEGORY('Axle keeper','Axle keeper',(#4969));
#4946=PRODUCT_RELATED_PRODUCT_CATEGORY('M4x10 Cap Screw',
'M4x10 Cap Screw',(#4970));
#4947=PRODUCT_RELATED_PRODUCT_CATEGORY('Wheel','Wheel',(#4971));
#4948=PRODUCT_RELATED_PRODUCT_CATEGORY(
'Wheel with twelve millimetre bearings',
'Wheel with twelve millimetre bearings',(#4972));
#4949=PRODUCT_RELATED_PRODUCT_CATEGORY(
'Sealed Ball Bearing - 12 x 32 x 10 mm',
'Sealed Ball Bearing - 12 x 32 x 10 mm',(#4973));
#4950=PRODUCT_RELATED_PRODUCT_CATEGORY('Inner ring','Inner ring',(#4974));
#4951=PRODUCT_RELATED_PRODUCT_CATEGORY('Outer ring','Outer ring',(#4975));
#4952=PRODUCT_RELATED_PRODUCT_CATEGORY('Balls','Balls',(#4976));
#4953=PRODUCT_RELATED_PRODUCT_CATEGORY('Cage','Cage',(#4977));
#4954=PRODUCT_RELATED_PRODUCT_CATEGORY('Seals 2RS','Seals 2RS',(#4978));
#4955=PRODUCT_RELATED_PRODUCT_CATEGORY('Bearing end retainer',
'Bearing end retainer',(#4979));
#4956=APPLICATION_PROTOCOL_DEFINITION('international standard',
'automotive_design',2009,#4957);
#4957=APPLICATION_CONTEXT(
'Core Data for Automotive Mechanical Design Process');
#4958=PRODUCT_CONTEXT('part definition',#4957,'mechanical');
#4959=PRODUCT('PAT-044','PAT-044',
'PAT-044',(#4958));
#4960=PRODUCT('Side frames axles and hanger',
'Side frames axles and hanger','Side frames axles and hanger',(#4958));
#4961=PRODUCT('Lower cross member','Lower cross member',
'Lower cross member',(#4958));
#4962=PRODUCT('Side frame plate','Side frame plate','Side frame plate',
(#4958));
#4963=PRODUCT('Welded eye plate','Welded eye plate','Welded eye plate',
(#4958));
#4964=PRODUCT('Flat Washer - M8','Flat Washer - M8','Flat Washer - M8',
(#4958));
#4965=PRODUCT('Cap Screw - M8x30','Cap Screw - M8x30',
'Cap Screw - M8x30',(#4958));
#4966=PRODUCT('Cantilever wheel axle','Cantilever wheel axle',
'Cantilever wheel axle',(#4958));
#4967=PRODUCT('Inner bearing spacer','Inner bearing spacer',
'Inner bearing spacer',(#4958));
#4968=PRODUCT('Outer bearing spacer','Outer bearing spacer',
'Outer bearing spacer',(#4958));
#4969=PRODUCT('Axle keeper','Axle keeper','Axle keeper',(#4958));
#4970=PRODUCT('M4x10 Cap Screw','M4x10 Cap Screw','M4x10 Cap Screw',(#4958));
#4971=PRODUCT('Wheel','Wheel','Wheel',(#4958));
#4972=PRODUCT('Wheel with twelve millimetre bearings',
'Wheel with twelve millimetre bearings',
'Wheel with twelve millimetre bearings',(#4958));
#4973=PRODUCT('Sealed Ball Bearing - 12 x 32 x 10 mm',
'Sealed Ball Bearing - 12 x 32 x 10 mm',
'Sealed Ball Bearing - 12 x 32 x 10 mm',(#4958));
#4974=PRODUCT('Inner ring','Inner ring','Inner ring',(#4958));
#4975=PRODUCT('Outer ring','Outer ring','Outer ring',(#4958));
#4976=PRODUCT('Balls','Balls','Balls',(#4958));
#4977=PRODUCT('Cage','Cage','Cage',(#4958));
#4978=PRODUCT('Seals 2RS','Seals 2RS','Seals 2RS',(#4958));
#4979=PRODUCT('Bearing end retainer','Bearing end retainer',
'Bearing end retainer',(#4958));
#4980=PRESENTATION_STYLE_ASSIGNMENT((#4987));
#4981=PRESENTATION_STYLE_ASSIGNMENT((#4988));
#4982=PRESENTATION_STYLE_ASSIGNMENT((#4989));
#4983=PRESENTATION_STYLE_ASSIGNMENT((#4990));
#4984=PRESENTATION_STYLE_ASSIGNMENT((#4991));
#4985=PRESENTATION_STYLE_ASSIGNMENT((#4992));
#4986=PRESENTATION_STYLE_ASSIGNMENT((#4993));
#4987=SURFACE_STYLE_USAGE(.BOTH.,#4994);
#4988=SURFACE_STYLE_USAGE(.BOTH.,#4995);
#4989=SURFACE_STYLE_USAGE(.BOTH.,#4996);
#4990=SURFACE_STYLE_USAGE(.BOTH.,#4997);
#4991=SURFACE_STYLE_USAGE(.BOTH.,#4998);
#4992=SURFACE_STYLE_USAGE(.BOTH.,#4999);
#4993=SURFACE_STYLE_USAGE(.BOTH.,#5000);
#4994=SURFACE_SIDE_STYLE('',(#5001));
#4995=SURFACE_SIDE_STYLE('',(#5002));
#4996=SURFACE_SIDE_STYLE('',(#5003));
#4997=SURFACE_SIDE_STYLE('',(#5004));
#4998=SURFACE_SIDE_STYLE('',(#5005));
#4999=SURFACE_SIDE_STYLE('',(#5006));
#5000=SURFACE_SIDE_STYLE('',(#5007));
#5001=SURFACE_STYLE_FILL_AREA(#5008);
#5002=SURFACE_STYLE_FILL_AREA(#5009);
#5003=SURFACE_STYLE_FILL_AREA(#5010);
#5004=SURFACE_STYLE_FILL_AREA(#5011);
#5005=SURFACE_STYLE_FILL_AREA(#5012);
#5006=SURFACE_STYLE_FILL_AREA(#5013);
#5007=SURFACE_STYLE_FILL_AREA(#5014);
#5008=FILL_AREA_STYLE('Steel - Satin',(#5015));
#5009=FILL_AREA_STYLE('CAD Library Painted - Engineering blue',(#5016));
#5010=FILL_AREA_STYLE('CAD Library Painted - Deep blue',(#5017));
#5011=FILL_AREA_STYLE('CAD Library Painted - Steel gray',(#5018));
#5012=FILL_AREA_STYLE('CAD Library Painted - Graphite',(#5019));
#5013=FILL_AREA_STYLE('CAD Library Painted - Light blue',(#5020));
#5014=FILL_AREA_STYLE('CAD Library Painted - Off white',(#5021));
#5015=FILL_AREA_STYLE_COLOUR('Steel - Satin',#5022);
#5016=FILL_AREA_STYLE_COLOUR('CAD Library Painted - Engineering blue',#5023);
#5017=FILL_AREA_STYLE_COLOUR('CAD Library Painted - Deep blue',#5024);
#5018=FILL_AREA_STYLE_COLOUR('CAD Library Painted - Steel gray',#5025);
#5019=FILL_AREA_STYLE_COLOUR('CAD Library Painted - Graphite',#5026);
#5020=FILL_AREA_STYLE_COLOUR('CAD Library Painted - Light blue',#5027);
#5021=FILL_AREA_STYLE_COLOUR('CAD Library Painted - Off white',#5028);
#5022=COLOUR_RGB('Steel - Satin',0.627450980392157,0.627450980392157,0.627450980392157);
#5023=COLOUR_RGB('CAD Library Painted - Engineering blue',0.12156862745098,
0.356862745098039,0.6);
#5024=COLOUR_RGB('CAD Library Painted - Deep blue',0.0784313725490196,0.203921568627451,
0.349019607843137);
#5025=COLOUR_RGB('CAD Library Painted - Steel gray',0.592156862745098,0.631372549019608,
0.67843137254902);
#5026=COLOUR_RGB('CAD Library Painted - Graphite',0.0980392156862745,0.109803921568627,
0.125490196078431);
#5027=COLOUR_RGB('CAD Library Painted - Light blue',0.286274509803922,0.552941176470588,
0.780392156862745);
#5028=COLOUR_RGB('CAD Library Painted - Off white',0.909803921568627,0.901960784313726,
0.858823529411765);
#5029=COLOUR_RGB('Dark Blue',0.08,0.2,0.34);
#5030=FILL_AREA_STYLE_COLOUR('',#5029);
#5031=FILL_AREA_STYLE('',(#5030));
#5032=SURFACE_STYLE_FILL_AREA(#5031);
#5033=SURFACE_SIDE_STYLE('',(#5032));
#5034=SURFACE_STYLE_USAGE(.BOTH.,#5033);
#5035=PRESENTATION_STYLE_ASSIGNMENT((#5034));
#5036=COLOUR_RGB('Light Blue',0.38,0.62,0.78);
#5037=FILL_AREA_STYLE_COLOUR('',#5036);
#5038=FILL_AREA_STYLE('',(#5037));
#5039=SURFACE_STYLE_FILL_AREA(#5038);
#5040=SURFACE_SIDE_STYLE('',(#5039));
#5041=SURFACE_STYLE_USAGE(.BOTH.,#5040);
#5042=PRESENTATION_STYLE_ASSIGNMENT((#5041));
#5043=COLOUR_RGB('Sky Blue',0.24,0.69,0.87);
#5044=FILL_AREA_STYLE_COLOUR('',#5043);
#5045=FILL_AREA_STYLE('',(#5044));
#5046=SURFACE_STYLE_FILL_AREA(#5045);
#5047=SURFACE_SIDE_STYLE('',(#5046));
#5048=SURFACE_STYLE_USAGE(.BOTH.,#5047);
#5049=PRESENTATION_STYLE_ASSIGNMENT((#5048));
#5050=COLOUR_RGB('Grey',0.48,0.52,0.57);
#5051=FILL_AREA_STYLE_COLOUR('',#5050);
#5052=FILL_AREA_STYLE('',(#5051));
#5053=SURFACE_STYLE_FILL_AREA(#5052);
#5054=SURFACE_SIDE_STYLE('',(#5053));
#5055=SURFACE_STYLE_USAGE(.BOTH.,#5054);
#5056=PRESENTATION_STYLE_ASSIGNMENT((#5055));
#5057=COLOUR_RGB('Black',0.12,0.14,0.17);
#5058=FILL_AREA_STYLE_COLOUR('',#5057);
#5059=FILL_AREA_STYLE('',(#5058));
#5060=SURFACE_STYLE_FILL_AREA(#5059);
#5061=SURFACE_SIDE_STYLE('',(#5060));
#5062=SURFACE_STYLE_USAGE(.BOTH.,#5061);
#5063=PRESENTATION_STYLE_ASSIGNMENT((#5062));
#5064=COLOUR_RGB('Off White',0.89,0.88,0.83);
#5065=FILL_AREA_STYLE_COLOUR('',#5064);
#5066=FILL_AREA_STYLE('',(#5065));
#5067=SURFACE_STYLE_FILL_AREA(#5066);
#5068=SURFACE_SIDE_STYLE('',(#5067));
#5069=SURFACE_STYLE_USAGE(.BOTH.,#5068);
#5070=PRESENTATION_STYLE_ASSIGNMENT((#5069));
ENDSEC;
END-ISO-10303-21;
